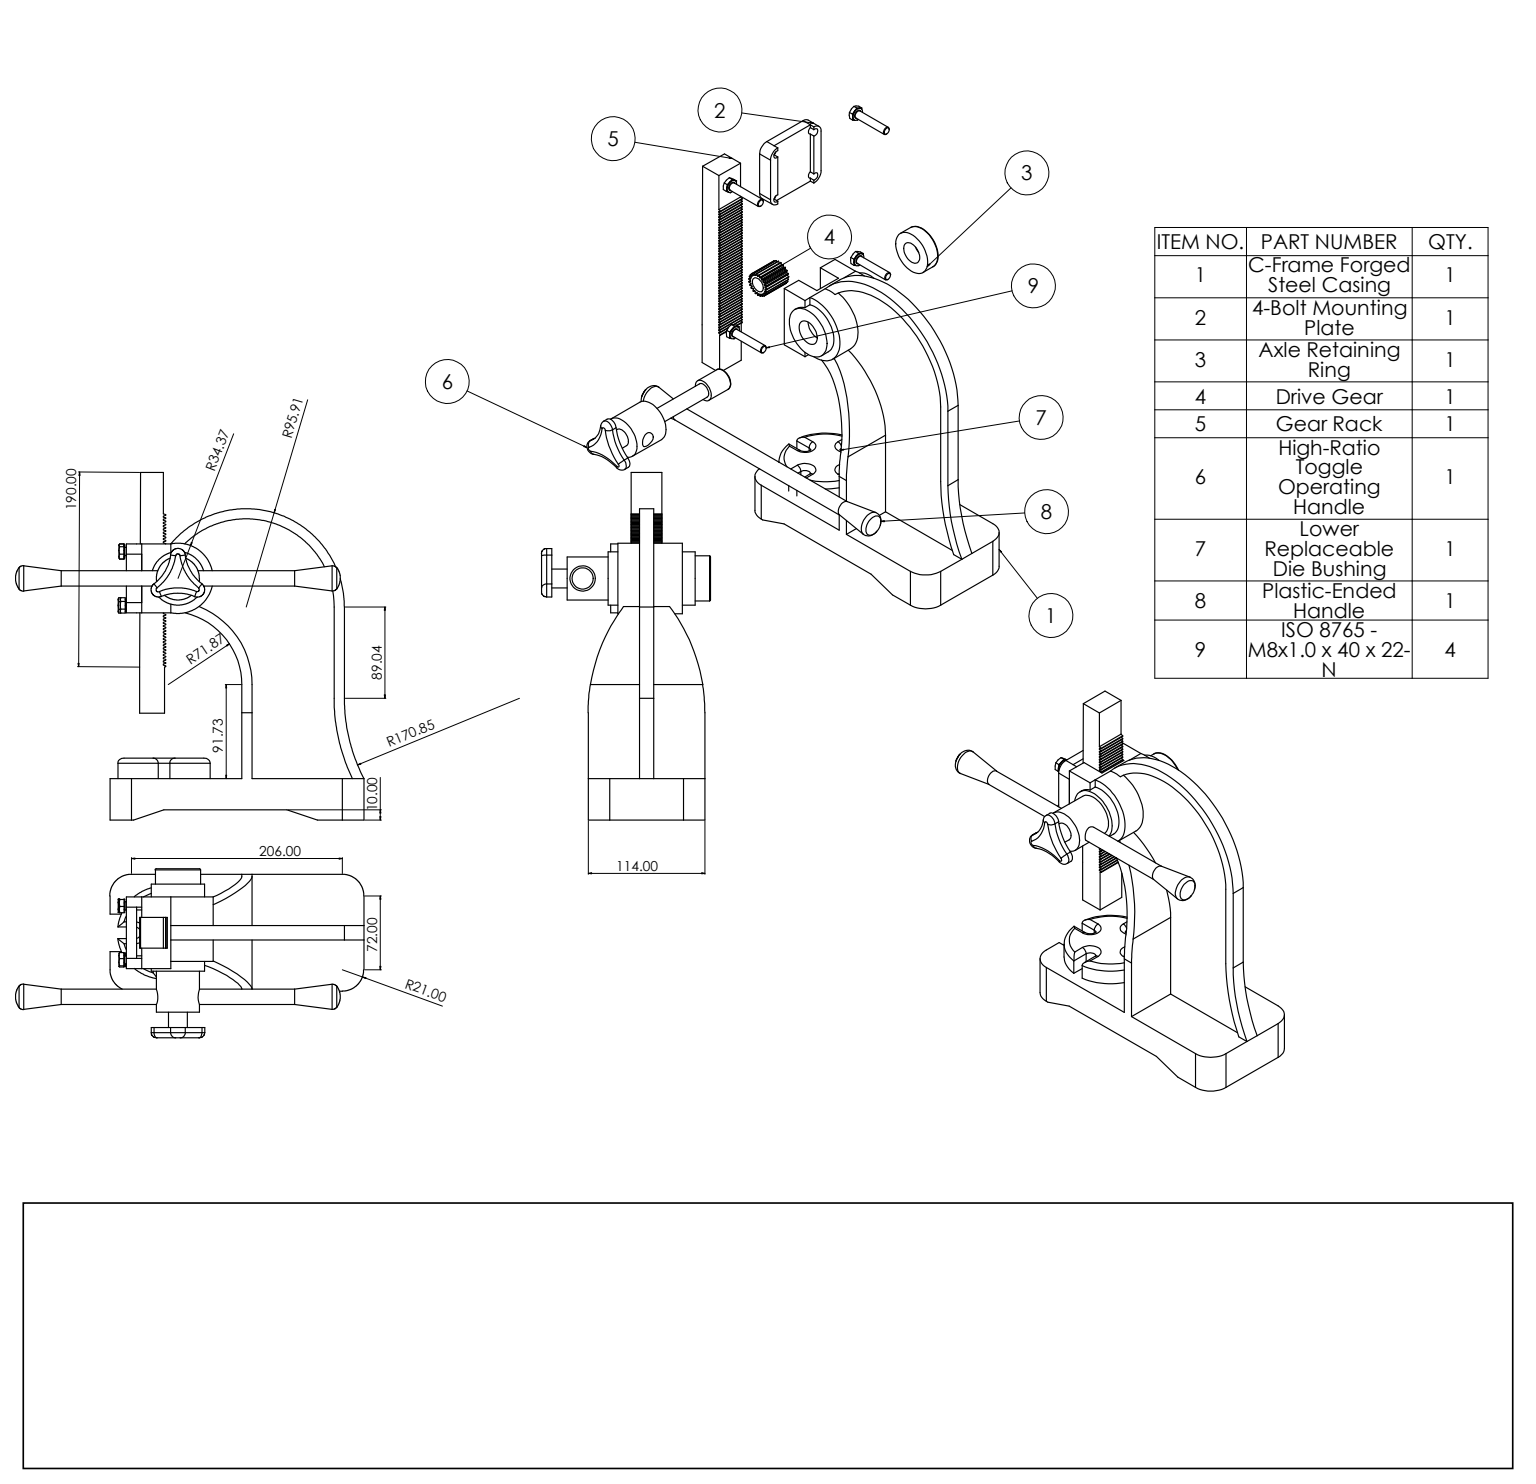
ISO-10303-21;
HEADER;
FILE_DESCRIPTION (('STEP AP214'),
    '1' );
FILE_NAME ('MAS-321',
    '2026-10-21T18:33:49',
    ( '' ),
    ( '' ),
    'SwSTEP 2.0',
    'SolidWorks 2025',
    '' );
FILE_SCHEMA (( 'AUTOMOTIVE_DESIGN' ));
ENDSEC;

DATA;
#1 = ORIENTED_EDGE ( 'NONE', *, *, #1823, .F. ) ;
#2 = EDGE_CURVE ( 'NONE', #15837, #10059, #9983, .T. ) ;
#3 = EDGE_CURVE ( 'NONE', #15101, #1867, #14100, .T. ) ;
#4 = VERTEX_POINT ( 'NONE', #5573 ) ;
#5 = DIRECTION ( 'NONE',  ( 0.000000000000000000, 1.000000000000000000, 0.000000000000000000 ) ) ;
#6 = CARTESIAN_POINT ( 'NONE',  ( 0.01372220897669153110, -5.309964801958256153, 3.802871176606155590 ) ) ;
#7 = CIRCLE ( 'NONE', #9259, 4.600000000000006750 ) ;
#8 = FACE_OUTER_BOUND ( 'NONE', #9764, .T. ) ;
#9 = EDGE_CURVE ( 'NONE', #4281, #6184, #12794, .T. ) ;
#10 = CARTESIAN_POINT ( 'NONE',  ( -68.99615306438082030, 67.98345733813023628, 15.00000000000006928 ) ) ;
#11 = AXIS2_PLACEMENT_3D ( 'NONE', #13563, #6445, #16272 ) ;
#12 = DIRECTION ( 'NONE',  ( -0.000000000000000000, -0.000000000000000000, -1.000000000000000000 ) ) ;
#13 = CIRCLE ( 'NONE', #606, 12.50000000000001776 ) ;
#14 = ORIENTED_EDGE ( 'NONE', *, *, #12006, .F. ) ;
#15 = ADVANCED_FACE ( 'NONE', ( #8489 ), #16983, .T. ) ;
#16 = DIRECTION ( 'NONE',  ( -5.204170427930409450E-16, 0.000000000000000000, 1.000000000000000000 ) ) ;
#17 = ORIENTED_EDGE ( 'NONE', *, *, #6060, .F. ) ;
#18 = CARTESIAN_POINT ( 'NONE',  ( -78.51801170372752381, -91.96846159163192169, 42.55230335834794175 ) ) ;
#19 = ADVANCED_FACE ( 'NONE', ( #15595 ), #11103, .T. ) ;
#20 = ADVANCED_FACE ( 'NONE', ( #8576 ), #7163, .T. ) ;
#21 = CARTESIAN_POINT ( 'NONE',  ( -67.50540723371459251, 87.07303407725210320, 15.00000000000006928 ) ) ;
#22 = ORIENTED_EDGE ( 'NONE', *, *, #922, .F. ) ;
#23 = VECTOR ( 'NONE', #5591, 1000.000000000000000 ) ;
#24 = CARTESIAN_POINT ( 'NONE',  ( -110.0337185876616815, -91.08930958056578220, -10.39386245929468444 ) ) ;
#25 = ORIENTED_EDGE ( 'NONE', *, *, #4430, .T. ) ;
#26 = AXIS2_PLACEMENT_3D ( 'NONE', #11599, #96, #9826 ) ;
#27 = ADVANCED_FACE ( 'NONE', ( #4362 ), #9999, .F. ) ;
#28 = VECTOR ( 'NONE', #11841, 1000.000000000000000 ) ;
#29 = VECTOR ( 'NONE', #2801, 1000.000000000000000 ) ;
#30 = EDGE_LOOP ( 'NONE', ( #4057, #14157, #6420, #5551 ) ) ;
#31 = SURFACE_STYLE_USAGE ( .BOTH. , #16764 ) ;
#32 = DIRECTION ( 'NONE',  ( -0.000000000000000000, -0.000000000000000000, -1.000000000000000000 ) ) ;
#33 = CARTESIAN_POINT ( 'NONE',  ( -68.99615306438083451, 95.64293533166268446, -15.00000000000001421 ) ) ;
#34 = ORIENTED_EDGE ( 'NONE', *, *, #18366, .F. ) ;
#35 = ITEM_DEFINED_TRANSFORMATION ( 'NONE', 'NONE', #15648,  #16217 ) ;
#36 = AXIS2_PLACEMENT_3D ( 'NONE', #1369, #138, #1266 ) ;
#37 = EDGE_LOOP ( 'NONE', ( #6433, #6306, #4816, #14039 ) ) ;
#38 = CARTESIAN_POINT ( 'NONE',  ( -27.30335599338096841, -92.58099833983887095, 7.070576347711331699 ) ) ;
#39 = DIRECTION ( 'NONE',  ( 3.469446951953611033E-15, 0.000000000000000000, -1.000000000000000000 ) ) ;
#40 = ORIENTED_EDGE ( 'NONE', *, *, #16480, .F. ) ;
#41 = LINE ( 'NONE', #15673, #2725 ) ;
#42 = DIRECTION ( 'NONE',  ( -1.000000000000000000, 5.416250486023790304E-15, 1.692578276882434470E-16 ) ) ;
#43 = CARTESIAN_POINT ( 'NONE',  ( -71.24615306438076345, 119.9567435045637609, 15.00000000000006928 ) ) ;
#44 = AXIS2_PLACEMENT_3D ( 'NONE', #11629, #14534, #15759 ) ;
#45 = AXIS2_PLACEMENT_3D ( 'NONE', #14996, #2189, #7901 ) ;
#46 = ORIENTED_EDGE ( 'NONE', *, *, #11434, .F. ) ;
#47 = EDGE_CURVE ( 'NONE', #3245, #18159, #14547, .T. ) ;
#48 = DIRECTION ( 'NONE',  ( -1.000000000000000000, 0.000000000000000000, 0.000000000000000000 ) ) ;
#49 = ORIENTED_EDGE ( 'NONE', *, *, #17445, .T. ) ;
#50 = ORIENTED_EDGE ( 'NONE', *, *, #8115, .F. ) ;
#51 = AXIS2_PLACEMENT_3D ( 'NONE', #16170, #17306, #13379 ) ;
#52 = DIRECTION ( 'NONE',  ( -1.000000000000000000, -0.000000000000000000, -0.000000000000000000 ) ) ;
#53 = ORIENTED_EDGE ( 'NONE', *, *, #16344, .F. ) ;
#54 = ORIENTED_EDGE ( 'NONE', *, *, #5988, .F. ) ;
#55 = CIRCLE ( 'NONE', #2439, 22.04359719766050318 ) ;
#56 = AXIS2_PLACEMENT_3D ( 'NONE', #11345, #9554, #17037 ) ;
#57 = DIRECTION ( 'NONE',  ( 0.000000000000000000, 0.000000000000000000, 1.000000000000000000 ) ) ;
#58 = DIRECTION ( 'NONE',  ( -1.000000000000000000, 0.000000000000000000, 1.156482317317869999E-16 ) ) ;
#59 = CARTESIAN_POINT ( 'NONE',  ( -71.24615306438080609, 110.5319655545637403, -15.00000000000001421 ) ) ;
#60 = VERTEX_POINT ( 'NONE', #5921 ) ;
#61 = CARTESIAN_POINT ( 'NONE',  ( -44.89980253466632831, 81.41924511788819530, 15.00000000000006928 ) ) ;
#62 = DIRECTION ( 'NONE',  ( 1.000000000000000000, 0.000000000000000000, 5.077734830647299712E-16 ) ) ;
#63 = CARTESIAN_POINT ( 'NONE',  ( -9.730036491473859073, 24.55694320255973651, 41.56001028271458608 ) ) ;
#64 = FACE_OUTER_BOUND ( 'NONE', #11864, .T. ) ;
#65 = ORIENTED_EDGE ( 'NONE', *, *, #13144, .F. ) ;
#66 = AXIS2_PLACEMENT_3D ( 'NONE', #17711, #16306, #507 ) ;
#67 = DIRECTION ( 'NONE',  ( 1.000000000000000000, 0.000000000000000000, 0.000000000000000000 ) ) ;
#68 = DIRECTION ( 'NONE',  ( 0.000000000000000000, 0.000000000000000000, -1.000000000000000000 ) ) ;
#69 = LINE ( 'NONE', #1924, #3643 ) ;
#70 = VERTEX_POINT ( 'NONE', #417 ) ;
#71 = CIRCLE ( 'NONE', #16786, 10.24900000000000055 ) ;
#72 = VECTOR ( 'NONE', #8079, 1000.000000000000000 ) ;
#73 = LINE ( 'NONE', #1738, #2546 ) ;
#74 = CARTESIAN_POINT ( 'NONE',  ( -71.24615306438114715, 12.25372266522925457, -15.00000000000001421 ) ) ;
#75 = CARTESIAN_POINT ( 'NONE',  ( -59.35080917176598092, 94.79374675277695417, -15.00000000000001421 ) ) ;
#76 = CARTESIAN_POINT ( 'NONE',  ( -68.99615306438099083, 39.70912348813027393, -15.00000000000001421 ) ) ;
#77 = ORIENTED_EDGE ( 'NONE', *, *, #12373, .F. ) ;
#78 = ORIENTED_EDGE ( 'NONE', *, *, #14054, .T. ) ;
#79 = VECTOR ( 'NONE', #3026, 1000.000000000000000 ) ;
#81 = ADVANCED_FACE ( 'NONE', ( #3143 ), #14460, .T. ) ;
#80 = FACE_OUTER_BOUND ( 'NONE', #8908, .T. ) ;
#82 = VECTOR ( 'NONE', #10770, 1000.000000000000000 ) ;
#83 = AXIS2_PLACEMENT_3D ( 'NONE', #305, #8649, #15842 ) ;
#84 = MANIFOLD_SOLID_BREP ( 'HeadFillet', #15945 ) ;
#85 =( NAMED_UNIT ( * ) SI_UNIT ( $, .STERADIAN. ) SOLID_ANGLE_UNIT ( ) );
#86 = CARTESIAN_POINT ( 'NONE',  ( -67.32681558843928826, 84.01587117655452630, 15.00000000000006928 ) ) ;
#87 = CARTESIAN_POINT ( 'NONE',  ( -71.24615306438086293, 87.65194626522927024, 15.00000000000006928 ) ) ;
#88 = CARTESIAN_POINT ( 'NONE',  ( -71.24615306438103346, 41.41692725456378099, 15.00000000000006928 ) ) ;
#89 = ORIENTED_EDGE ( 'NONE', *, *, #17144, .T. ) ;
#90 = DIRECTION ( 'NONE',  ( -0.000000000000000000, 0.000000000000000000, -1.000000000000000000 ) ) ;
#91 = LINE ( 'NONE', #5786, #7353 ) ;
#92 = FACE_OUTER_BOUND ( 'NONE', #4705, .T. ) ;
#93 = ORIENTED_EDGE ( 'NONE', *, *, #600, .F. ) ;
#94 = DIRECTION ( 'NONE',  ( 1.000000000000000000, 0.000000000000000000, -0.000000000000000000 ) ) ;
#95 = AXIS2_PLACEMENT_3D ( 'NONE', #13870, #16563, #957 ) ;
#96 = DIRECTION ( 'NONE',  ( -1.000000000000000000, -0.000000000000000000, -0.000000000000000000 ) ) ;
#97 = EDGE_LOOP ( 'NONE', ( #14559, #13719, #17905, #14362 ) ) ;
#98 = VECTOR ( 'NONE', #835, 1000.000000000000000 ) ;
#99 = CARTESIAN_POINT ( 'NONE',  ( -57.08002265617300708, 84.22855780814606419, 35.00000000000000000 ) ) ;
#100 = VECTOR ( 'NONE', #7999, 1000.000000000000000 ) ;
#101 = CARTESIAN_POINT ( 'NONE',  ( -71.24615306438103346, 46.81124181522922356, -167.1454815528550739 ) ) ;
#102 = ORIENTED_EDGE ( 'NONE', *, *, #5033, .T. ) ;
#103 = VERTEX_POINT ( 'NONE', #8932 ) ;
#104 = VECTOR ( 'NONE', #14107, 1000.000000000000000 ) ;
#105 = EDGE_CURVE ( 'NONE', #6184, #7713, #7257, .T. ) ;
#106 = DIRECTION ( 'NONE',  ( 0.000000000000000000, 0.000000000000000000, 1.000000000000000000 ) ) ;
#107 = CARTESIAN_POINT ( 'NONE',  ( -68.99615306438077766, 111.3508985816626335, 15.00000000000006928 ) ) ;
#108 = DIRECTION ( 'NONE',  ( 0.9396926207859110924, 0.3420201433256612189, 4.890320548438462711E-16 ) ) ;
#109 = CARTESIAN_POINT ( 'NONE',  ( -68.99615306438083451, 96.25779118813026969, 15.00000000000006928 ) ) ;
#110 = AXIS2_PLACEMENT_3D ( 'NONE', #2783, #3985, #15597 ) ;
#111 = AXIS2_PLACEMENT_3D ( 'NONE', #807, #12215, #17823 ) ;
#112 = CARTESIAN_POINT ( 'NONE',  ( -68.99615306438094819, 64.84186468813030046, -167.1454815528550739 ) ) ;
#113 = VERTEX_POINT ( 'NONE', #1813 ) ;
#114 = CARTESIAN_POINT ( 'NONE',  ( -57.08002265617300708, 84.22855780814606419, 15.00000000000006928 ) ) ;
#115 = VERTEX_POINT ( 'NONE', #11567 ) ;
#116 = EDGE_CURVE ( 'NONE', #6374, #8001, #17153, .T. ) ;
#117 = DIRECTION ( 'NONE',  ( 0.000000000000000000, 1.000000000000000000, -0.000000000000000000 ) ) ;
#118 = DIRECTION ( 'NONE',  ( 0.000000000000000000, -0.000000000000000000, 1.000000000000000000 ) ) ;
#120 = ADVANCED_FACE ( 'NONE', ( #317 ), #17523, .T. ) ;
#119 = ORIENTED_EDGE ( 'NONE', *, *, #16367, .F. ) ;
#121 = CARTESIAN_POINT ( 'NONE',  ( -115.7702289486887537, -95.65021661331556402, -5.654315315326000402 ) ) ;
#122 = ORIENTED_EDGE ( 'NONE', *, *, #17197, .T. ) ;
#123 = EDGE_CURVE ( 'NONE', #14184, #1161, #17431, .T. ) ;
#124 = AXIS2_PLACEMENT_3D ( 'NONE', #9916, #7194, #14307 ) ;
#125 = AXIS2_PLACEMENT_3D ( 'NONE', #2638, #18365, #4052 ) ;
#126 = ADVANCED_FACE ( 'NONE', ( #11640 ), #16856, .T. ) ;
#127 = ORIENTED_EDGE ( 'NONE', *, *, #11107, .F. ) ;
#128 = EDGE_CURVE ( 'NONE', #7354, #7590, #10341, .T. ) ;
#129 = FACE_OUTER_BOUND ( 'NONE', #15736, .T. ) ;
#130 = CYLINDRICAL_SURFACE ( 'NONE', #6082, 21.04359719766050318 ) ;
#131 = DIRECTION ( 'NONE',  ( 0.000000000000000000, 1.000000000000000000, 0.000000000000000000 ) ) ;
#132 = CLOSED_SHELL ( 'NONE', ( #16819, #11674, #2033, #11644, #4371, #4122, #1296, #5932, #17847, #120, #2885, #7783, #14078, #8551, #16458, #7777, #18333, #11455, #10717, #14761, #5893, #8655, #18440, #16557, #12743, #9060, #2113, #2878, #10557, #2402, #8018, #1483, #10883, #4144, #6355, #12130, #16320, #4815, #13864, #11004, #16568, #13389, #1952, #7426, #15874, #4708, #2702, #9166, #6647, #9938, #17322, #16215, #6855, #13752, #18352, #9497, #4258, #1742, #6653, #8457, #4789, #9269, #18511, #11812, #1620, #13520, #17365, #6946, #1859, #1613, #14320, #1393, #8249, #8120, #5145, #15892, #8683, #10886, #4488, #15641, #15634, #1683, #17355, #13695, #2863, #11359, #9380, #16584, #2602, #1587, #18091, #10091, #697, #5265, #11665, #1664, #1494, #15112, #7329, #13942, #12957, #5269, #13366, #4588, #17837, #11471, #8147, #8734, #4244, #11669, #7993, #15996, #11378, #16587, #15586, #9173, #1719, #9985, #9137, #3228, #3620, #3217, #7092, #3899, #10422, #4564, #11884, #18090, #10942, #9980, #5134, #5026, #2281, #4013, #13406, #12017, #13887, #8689, #14413, #199, #11412, #7110, #12033, #2993, #2286, #360, #17572, #10733, #12952, #12754, #9744, #1961, #13863, #8387, #17357, #7212, #8267, #16341, #10832, #3777, #7577, #14524, #13388, #3293, #4798, #16330, #4522, #14219, #18302, #4015, #3342, #248, #17345, #4135, #15214, #12844, #9850, #14995, #14426, #12814, #8137, #5256, #5374, #4240, #691, #4541, #672, #7328, #12390, #3982, #7563, #1284, #2154, #15527, #5570, #7390, #1348, #13976, #16311 ) ) ;
#133 = ORIENTED_EDGE ( 'NONE', *, *, #16066, .F. ) ;
#134 = CONTEXT_DEPENDENT_SHAPE_REPRESENTATION ( #8503, #15053 ) ;
#135 = ORIENTED_EDGE ( 'NONE', *, *, #18293, .T. ) ;
#136 = VECTOR ( 'NONE', #9589, 1000.000000000000000 ) ;
#137 = EDGE_CURVE ( 'NONE', #18033, #6955, #3220, .T. ) ;
#138 = DIRECTION ( 'NONE',  ( -0.000000000000000000, -0.000000000000000000, -1.000000000000000000 ) ) ;
#139 = CARTESIAN_POINT ( 'NONE',  ( -127.5926225674731711, 57.88796029049329661, -26.35917033480641436 ) ) ;
#140 = EDGE_CURVE ( 'NONE', #5342, #10434, #506, .T. ) ;
#141 = AXIS2_PLACEMENT_3D ( 'NONE', #1798, #14535, #303 ) ;
#142 = CARTESIAN_POINT ( 'NONE',  ( -71.24615306438106188, 35.13374195456378146, 15.00000000000006928 ) ) ;
#143 = CIRCLE ( 'NONE', #12708, 3.999999999999996447 ) ;
#144 = ADVANCED_FACE ( 'NONE', ( #11916 ), #17609, .T. ) ;
#145 = EDGE_LOOP ( 'NONE', ( #17261, #13971, #8851, #5219 ) ) ;
#146 = VECTOR ( 'NONE', #7240, 1000.000000000000114 ) ;
#147 = DIRECTION ( 'NONE',  ( 1.156482317317869999E-16, 0.000000000000000000, 1.000000000000000000 ) ) ;
#148 = ORIENTED_EDGE ( 'NONE', *, *, #2746, .F. ) ;
#149 = ORIENTED_EDGE ( 'NONE', *, *, #11735, .T. ) ;
#150 = EDGE_CURVE ( 'NONE', #4219, #3665, #3494, .T. ) ;
#151 = COLOUR_RGB ( '',0.7921568627450980005, 0.8196078431372548767, 0.9333333333333333481 ) ;
#152 = MANIFOLD_SOLID_BREP ( 'Revolve1', #15042 ) ;
#153 = ORIENTED_EDGE ( 'NONE', *, *, #7643, .F. ) ;
#154 = AXIS2_PLACEMENT_3D ( 'NONE', #13342, #6302, #517 ) ;
#155 = AXIS2_PLACEMENT_3D ( 'NONE', #551, #8645, #16166 ) ;
#156 = EDGE_CURVE ( 'NONE', #14603, #10461, #7800, .T. ) ;
#157 = CIRCLE ( 'NONE', #3134, 10.38004356723770627 ) ;
#158 = DIRECTION ( 'NONE',  ( 0.000000000000000000, 0.000000000000000000, -1.000000000000000000 ) ) ;
#159 = EDGE_CURVE ( 'NONE', #3245, #14275, #15961, .T. ) ;
#160 = CARTESIAN_POINT ( 'NONE',  ( -68.99615306438087714, 64.84186468813027204, 15.00000000000006928 ) ) ;
#161 = LINE ( 'NONE', #5851, #4306 ) ;
#162 = VERTEX_POINT ( 'NONE', #5272 ) ;
#163 = CARTESIAN_POINT ( 'NONE',  ( -71.24615306438072082, 129.3815214545637104, -15.00000000000001421 ) ) ;
#164 = DIRECTION ( 'NONE',  ( -1.000000000000000000, 0.000000000000000000, 0.000000000000000000 ) ) ;
#165 = DIRECTION ( 'NONE',  ( 0.000000000000000000, 1.000000000000000000, 0.000000000000000000 ) ) ;
#166 = PLANE ( 'NONE',  #9698 ) ;
#167 = ORIENTED_EDGE ( 'NONE', *, *, #3319, .T. ) ;
#168 = DIRECTION ( 'NONE',  ( 0.000000000000000000, -1.000000000000000000, 0.000000000000000000 ) ) ;
#169 = CARTESIAN_POINT ( 'NONE',  ( -59.35080917176598092, 94.79374675277695417, 15.00000000000006928 ) ) ;
#170 = FACE_OUTER_BOUND ( 'NONE', #6777, .T. ) ;
#171 = EDGE_LOOP ( 'NONE', ( #9125, #326, #2269 ) ) ;
#172 = VECTOR ( 'NONE', #13804, 1000.000000000000000 ) ;
#173 = VECTOR ( 'NONE', #14749, 1000.000000000000000 ) ;
#174 = VECTOR ( 'NONE', #6629, 999.9999999999998863 ) ;
#175 = DIRECTION ( 'NONE',  ( 1.000000000000000000, 0.000000000000000000, 0.000000000000000000 ) ) ;
#176 = DIRECTION ( 'NONE',  ( 0.000000000000000000, 1.000000000000000000, 0.000000000000000000 ) ) ;
#177 = ORIENTED_EDGE ( 'NONE', *, *, #14769, .T. ) ;
#178 = EDGE_LOOP ( 'NONE', ( #16402, #10742, #3348, #2661 ) ) ;
#179 = DIRECTION ( 'NONE',  ( 1.000000000000000000, 0.000000000000000000, 5.551115123125780730E-16 ) ) ;
#180 = CIRCLE ( 'NONE', #10627, 4.025000000000000355 ) ;
#181 = SHAPE_REPRESENTATION_RELATIONSHIP ( 'NONE' , 'NONE' ,  #5501, #12175 ) ;
#182 = VECTOR ( 'NONE', #7830, 1000.000000000000000 ) ;
#183 = CARTESIAN_POINT ( 'NONE',  ( -70.85175816390371040, -141.5628872026273086, -18.23991632971910803 ) ) ;
#184 = CARTESIAN_POINT ( 'NONE',  ( -64.80066835027049876, -94.42547236494613117, -44.74948972093426391 ) ) ;
#185 = ORIENTED_EDGE ( 'NONE', *, *, #7525, .T. ) ;
#186 = CARTESIAN_POINT ( 'NONE',  ( 49.38736944425944841, -141.5628872026273086, -57.00000000000000000 ) ) ;
#187 = DIRECTION ( 'NONE',  ( -5.204170427930409450E-16, 0.000000000000000000, 1.000000000000000000 ) ) ;
#188 = DIRECTION ( 'NONE',  ( 0.000000000000000000, 0.000000000000000000, 1.000000000000000000 ) ) ;
#189 = DIRECTION ( 'NONE',  ( -0.9396926207859084279, 0.3420201433256686574, -4.890320548438448905E-16 ) ) ;
#190 = ORIENTED_EDGE ( 'NONE', *, *, #16753, .F. ) ;
#191 = DIRECTION ( 'NONE',  ( 1.156482317317869999E-16, 0.000000000000000000, 1.000000000000000000 ) ) ;
#192 = CYLINDRICAL_SURFACE ( 'NONE', #914, 11.04359719766050141 ) ;
#193 = EDGE_LOOP ( 'NONE', ( #119, #17076, #7928, #5091 ) ) ;
#194 = PRODUCT_RELATED_PRODUCT_CATEGORY ( 'part', '', ( #10574 ) ) ;
#195 = CYLINDRICAL_SURFACE ( 'NONE', #16432, 4.599999999999999645 ) ;
#196 = CARTESIAN_POINT ( 'NONE',  ( -93.73308511844572877, 147.7866419848965052, 15.00000000000006928 ) ) ;
#197 = VERTEX_POINT ( 'NONE', #9569 ) ;
#198 = ORIENTED_EDGE ( 'NONE', *, *, #17480, .F. ) ;
#199 = ADVANCED_FACE ( 'NONE', ( #6677 ), #6475, .T. ) ;
#200 = ORIENTED_EDGE ( 'NONE', *, *, #18072, .T. ) ;
#201 = DIRECTION ( 'NONE',  ( -1.000000000000000000, 2.331468351712825579E-14, 1.387778780781443703E-16 ) ) ;
#202 = LINE ( 'NONE', #14676, #5765 ) ;
#203 = FACE_OUTER_BOUND ( 'NONE', #17910, .T. ) ;
#204 = FACE_OUTER_BOUND ( 'NONE', #12195, .T. ) ;
#205 = CARTESIAN_POINT ( 'NONE',  ( -64.09025127992788384, 50.58224449241410525, 35.00000000000000000 ) ) ;
#206 = ORIENTED_EDGE ( 'NONE', *, *, #10760, .F. ) ;
#207 = CARTESIAN_POINT ( 'NONE',  ( -68.99615306438072082, 139.6252324316626812, -15.00000000000001421 ) ) ;
#208 = CARTESIAN_POINT ( 'NONE',  ( -80.32997185471272417, -91.18731257919070288, 40.31990080433438095 ) ) ;
#209 = DIRECTION ( 'NONE',  ( 1.156482317317869999E-16, 0.000000000000000000, 1.000000000000000000 ) ) ;
#210 = ORIENTED_EDGE ( 'NONE', *, *, #16102, .F. ) ;
#211 = CARTESIAN_POINT ( 'NONE',  ( -71.24615306438094819, 65.66079771522920794, 15.00000000000006928 ) ) ;
#212 = CARTESIAN_POINT ( 'NONE',  ( -114.8884567811962967, -93.39009998357855125, -6.425136209964025902 ) ) ;
#213 = ORIENTED_EDGE ( 'NONE', *, *, #3679, .F. ) ;
#214 = EDGE_LOOP ( 'NONE', ( #597, #4033, #2043, #6029 ) ) ;
#215 = ADVANCED_FACE ( 'NONE', ( #695 ), #10288, .T. ) ;
#216 = DIRECTION ( 'NONE',  ( 0.000000000000000000, 0.000000000000000000, 1.000000000000000000 ) ) ;
#217 = CARTESIAN_POINT ( 'NONE',  ( -97.59262256747317110, 0.3328663868096687350, 25.00000000000000000 ) ) ;
#218 = DIRECTION ( 'NONE',  ( 0.000000000000000000, 0.000000000000000000, 1.000000000000000000 ) ) ;
#219 = ORIENTED_EDGE ( 'NONE', *, *, #12477, .T. ) ;
#220 = ORIENTED_EDGE ( 'NONE', *, *, #11450, .F. ) ;
#221 = CARTESIAN_POINT ( 'NONE',  ( -81.37409655828265898, -96.08423613455721579, -2.623087607583323579E-13 ) ) ;
#222 = FACE_OUTER_BOUND ( 'NONE', #11208, .T. ) ;
#223 = DIRECTION ( 'NONE',  ( 0.000000000000000000, -0.000000000000000000, 1.000000000000000000 ) ) ;
#224 = CARTESIAN_POINT ( 'NONE',  ( -68.99615306438066398, 143.3816809381303585, -15.00000000000001421 ) ) ;
#225 = ORIENTED_EDGE ( 'NONE', *, *, #7011, .F. ) ;
#226 = EDGE_CURVE ( 'NONE', #10713, #3636, #7893, .T. ) ;
#227 = DIRECTION ( 'NONE',  ( 1.000000000000000000, 0.000000000000000000, 0.000000000000000000 ) ) ;
#228 = ORIENTED_EDGE ( 'NONE', *, *, #586, .F. ) ;
#229 = EDGE_CURVE ( 'NONE', #6748, #3936, #16550, .T. ) ;
#230 = EDGE_LOOP ( 'NONE', ( #6684, #5867, #2533, #3953 ) ) ;
#231 = ORIENTED_EDGE ( 'NONE', *, *, #17262, .F. ) ;
#232 = EDGE_CURVE ( 'NONE', #7225, #15152, #10982, .T. ) ;
#233 = EDGE_CURVE ( 'NONE', #4074, #17713, #2000, .T. ) ;
#234 = DIRECTION ( 'NONE',  ( 0.000000000000000000, 0.000000000000000000, 1.000000000000000000 ) ) ;
#235 = CARTESIAN_POINT ( 'NONE',  ( -68.99615306438097662, 57.94382353166266597, 15.00000000000006928 ) ) ;
#236 = ORIENTED_EDGE ( 'NONE', *, *, #5271, .F. ) ;
#237 = CYLINDRICAL_SURFACE ( 'NONE', #286, 4.599999999999999645 ) ;
#238 = CARTESIAN_POINT ( 'NONE',  ( -68.99615306438094819, 52.27549408813023746, -15.00000000000001421 ) ) ;
#239 = CARTESIAN_POINT ( 'NONE',  ( -68.99615306438091977, 76.79337943166271430, 15.00000000000006928 ) ) ;
#240 = DIRECTION ( 'NONE',  ( 1.000000000000000000, 0.000000000000000000, 0.000000000000000000 ) ) ;
#241 = ORIENTED_EDGE ( 'NONE', *, *, #15088, .F. ) ;
#242 = EDGE_CURVE ( 'NONE', #13281, #15993, #13414, .T. ) ;
#243 = CARTESIAN_POINT ( 'NONE',  ( 0.000000000000000000, -47.21335801510345220, 0.000000000000000000 ) ) ;
#244 = EDGE_CURVE ( 'NONE', #4575, #11504, #16586, .T. ) ;
#245 = DIRECTION ( 'NONE',  ( 0.000000000000000000, 1.000000000000000000, 0.000000000000000000 ) ) ;
#246 = CARTESIAN_POINT ( 'NONE',  ( -68.99615306438089135, 67.36860148166267948, -15.00000000000001421 ) ) ;
#247 = EDGE_LOOP ( 'NONE', ( #1699, #2209, #13687, #4336 ) ) ;
#248 = ADVANCED_FACE ( 'NONE', ( #16665 ), #17710, .T. ) ;
#249 = CYLINDRICAL_SURFACE ( 'NONE', #1928, 10.24900000000000766 ) ;
#250 = EDGE_CURVE ( 'NONE', #2407, #15787, #4070, .T. ) ;
#251 = AXIS2_PLACEMENT_3D ( 'NONE', #13885, #4066, #1079 ) ;
#252 = DIRECTION ( 'NONE',  ( 0.000000000000000000, 0.000000000000000000, 1.000000000000000000 ) ) ;
#253 = EDGE_LOOP ( 'NONE', ( #10457, #6808, #9246, #11912 ) ) ;
#254 = EDGE_LOOP ( 'NONE', ( #4957, #10703, #17741, #2803 ) ) ;
#255 = EDGE_CURVE ( 'NONE', #17238, #6285, #13006, .T. ) ;
#256 = DIRECTION ( 'NONE',  ( 0.000000000000000000, 0.000000000000000000, 1.000000000000000000 ) ) ;
#257 = MANIFOLD_SOLID_BREP ( 'Fillet4', #11497 ) ;
#258 = DIRECTION ( 'NONE',  ( 1.000000000000000000, 0.000000000000000000, 0.000000000000000000 ) ) ;
#259 = CARTESIAN_POINT ( 'NONE',  ( -49.58002265617300708, 84.22855780814606419, 35.00000000000000000 ) ) ;
#260 = DIRECTION ( 'NONE',  ( 1.000000000000000000, 0.000000000000000000, 0.000000000000000000 ) ) ;
#261 = VECTOR ( 'NONE', #17294, 1000.000000000000000 ) ;
#262 = CARTESIAN_POINT ( 'NONE',  ( -92.59262256747321373, 107.8748711238780373, 25.00000000000000000 ) ) ;
#263 = ORIENTED_EDGE ( 'NONE', *, *, #18181, .T. ) ;
#264 = CYLINDRICAL_SURFACE ( 'NONE', #16430, 21.04359719766050318 ) ;
#265 = DIRECTION ( 'NONE',  ( 0.000000000000000000, 0.000000000000000000, 1.000000000000000000 ) ) ;
#266 = CARTESIAN_POINT ( 'NONE',  ( -37.39678785461407529, 56.02900023377289074, 23.03959524935876857 ) ) ;
#267 = CARTESIAN_POINT ( 'NONE',  ( -38.92363814577095837, 71.26406042838981136, 102.5000000000000000 ) ) ;
#268 = DIRECTION ( 'NONE',  ( -0.000000000000000000, -0.000000000000000000, -1.000000000000000000 ) ) ;
#269 = DIRECTION ( 'NONE',  ( 0.000000000000000000, -2.775557561562874095E-16, 1.000000000000000000 ) ) ;
#270 = ORIENTED_EDGE ( 'NONE', *, *, #16707, .F. ) ;
#271 = CARTESIAN_POINT ( 'NONE',  ( -66.92930002414082935, 60.44851893123529152, 25.00000000000000000 ) ) ;
#272 = CARTESIAN_POINT ( 'NONE',  ( -67.13262496892538422, 91.65790412808873100, -167.1454815528550739 ) ) ;
#273 = ORIENTED_EDGE ( 'NONE', *, *, #7918, .F. ) ;
#274 = VERTEX_POINT ( 'NONE', #11460 ) ;
#275 = ORIENTED_EDGE ( 'NONE', *, *, #8832, .T. ) ;
#276 = LINE ( 'NONE', #12841, #12086 ) ;
#277 = CARTESIAN_POINT ( 'NONE',  ( -71.24615306438070661, 137.9174286652292096, -15.00000000000001421 ) ) ;
#278 = CARTESIAN_POINT ( 'NONE',  ( -68.99615306438091977, 76.79337943166271430, 15.00000000000006928 ) ) ;
#279 = DIRECTION ( 'NONE',  ( -0.9396926207859097602, 0.3420201433256649937, 1.086737899652991371E-16 ) ) ;
#280 = CARTESIAN_POINT ( 'NONE',  ( -93.73308511844572877, 147.7866419848965052, -167.1454815528550739 ) ) ;
#281 = CARTESIAN_POINT ( 'NONE',  ( -71.24615306438117557, 2.828944715229236628, -15.00000000000001421 ) ) ;
#282 = ORIENTED_EDGE ( 'NONE', *, *, #10987, .T. ) ;
#283 = AXIS2_PLACEMENT_3D ( 'NONE', #4428, #227, #10141 ) ;
#284 = DIRECTION ( 'NONE',  ( 0.000000000000000000, 0.000000000000000000, 1.000000000000000000 ) ) ;
#285 = CARTESIAN_POINT ( 'NONE',  ( -80.85270481229034090, -91.10977358899566525, 39.65137850708985923 ) ) ;
#286 = AXIS2_PLACEMENT_3D ( 'NONE', #17181, #15858, #14286 ) ;
#287 = CARTESIAN_POINT ( 'NONE',  ( -71.24615306438091977, 78.22716831522920700, -167.1454815528550739 ) ) ;
#288 = VERTEX_POINT ( 'NONE', #1257 ) ;
#289 = LINE ( 'NONE', #11809, #4058 ) ;
#290 = DIRECTION ( 'NONE',  ( 0.000000000000000000, 1.000000000000000000, -0.000000000000000000 ) ) ;
#291 = ORIENTED_EDGE ( 'NONE', *, *, #13628, .T. ) ;
#292 = VECTOR ( 'NONE', #17881, 1000.000000000000000 ) ;
#293 = VERTEX_POINT ( 'NONE', #8174 ) ;
#294 = AXIS2_PLACEMENT_3D ( 'NONE', #10449, #2985, #15881 ) ;
#295 = DIRECTION ( 'NONE',  ( 1.000000000000000000, 0.000000000000000000, 3.771137991253934490E-16 ) ) ;
#296 = LINE ( 'NONE', #5733, #146 ) ;
#297 = EDGE_CURVE ( 'NONE', #9307, #9072, #17170, .T. ) ;
#298 = LINE ( 'NONE', #4419, #17998 ) ;
#299 = VERTEX_POINT ( 'NONE', #17149 ) ;
#300 = ORIENTED_EDGE ( 'NONE', *, *, #349, .T. ) ;
#301 = DIRECTION ( 'NONE',  ( 0.000000000000000000, 0.000000000000000000, -1.000000000000000000 ) ) ;
#302 = CARTESIAN_POINT ( 'NONE',  ( 105.4583593777967963, -32.62665103886256190, -7.000000000000010658 ) ) ;
#303 = DIRECTION ( 'NONE',  ( -0.9396926207859083169, 0.3420201433256687129, 0.000000000000000000 ) ) ;
#304 = VECTOR ( 'NONE', #7741, 1000.000000000000000 ) ;
#305 = CARTESIAN_POINT ( 'NONE',  ( -56.26901274438541378, 73.45256821284058901, -15.00000000000001421 ) ) ;
#306 = ORIENTED_EDGE ( 'NONE', *, *, #1227, .F. ) ;
#307 = CIRCLE ( 'NONE', #13165, 4.962965561209093046 ) ;
#308 = PLANE ( 'NONE',  #11935 ) ;
#309 = EDGE_CURVE ( 'NONE', #9564, #16752, #11785, .T. ) ;
#310 = ORIENTED_EDGE ( 'NONE', *, *, #17032, .T. ) ;
#311 = EDGE_CURVE ( 'NONE', #17138, #8972, #12775, .T. ) ;
#312 = AXIS2_PLACEMENT_3D ( 'NONE', #18500, #6897, #18319 ) ;
#313 = ORIENTED_EDGE ( 'NONE', *, *, #10756, .F. ) ;
#314 = MANIFOLD_SOLID_BREP ( 'Cut-Extrude8', #12995 ) ;
#315 = VERTEX_POINT ( 'NONE', #4152 ) ;
#316 = VECTOR ( 'NONE', #2722, 1000.000000000000000 ) ;
#317 = FACE_OUTER_BOUND ( 'NONE', #5144, .T. ) ;
#318 = AXIS2_PLACEMENT_3D ( 'NONE', #739, #6431, #16426 ) ;
#319 = FACE_BOUND ( 'NONE', #1203, .T. ) ;
#320 = LINE ( 'NONE', #12982, #15345 ) ;
#321 = EDGE_LOOP ( 'NONE', ( #11496, #14503 ) ) ;
#322 = AXIS2_PLACEMENT_3D ( 'NONE', #3585, #3405, #3694 ) ;
#323 = DIRECTION ( 'NONE',  ( 0.000000000000000000, 0.000000000000000000, -1.000000000000000000 ) ) ;
#324 = FACE_OUTER_BOUND ( 'NONE', #5532, .T. ) ;
#325 = CARTESIAN_POINT ( 'NONE',  ( -69.66239992860627694, 84.22855780814606419, 37.50000000000000000 ) ) ;
#326 = ORIENTED_EDGE ( 'NONE', *, *, #2755, .T. ) ;
#327 = CARTESIAN_POINT ( 'NONE',  ( -71.24615306438086293, 101.1071876045637055, 15.00000000000006928 ) ) ;
#328 = CYLINDRICAL_SURFACE ( 'NONE', #16782, 4.599999999999999645 ) ;
#329 = DIRECTION ( 'NONE',  ( 1.156482317317869999E-16, 0.000000000000000000, 1.000000000000000000 ) ) ;
#330 = ORIENTED_EDGE ( 'NONE', *, *, #16668, .T. ) ;
#331 = EDGE_CURVE ( 'NONE', #1479, #11856, #14263, .T. ) ;
#332 = AXIS2_PLACEMENT_3D ( 'NONE', #14799, #4971, #14887 ) ;
#333 = EDGE_CURVE ( 'NONE', #677, #12056, #6961, .T. ) ;
#334 = CARTESIAN_POINT ( 'NONE',  ( -107.5926225674731853, 110.5691553257988460, 22.33417033480641223 ) ) ;
#335 = EDGE_CURVE ( 'NONE', #5779, #10128, #2839, .T. ) ;
#336 = CARTESIAN_POINT ( 'NONE',  ( 0.000000000000000000, -111.0842361345572158, 0.000000000000000000 ) ) ;
#337 = AXIS2_PLACEMENT_3D ( 'NONE', #17527, #14630, #13242 ) ;
#338 = ORIENTED_EDGE ( 'NONE', *, *, #1743, .T. ) ;
#339 = ORIENTED_EDGE ( 'NONE', *, *, #18046, .F. ) ;
#340 = ADVANCED_FACE ( 'NONE', ( #13312 ), #13217, .T. ) ;
#341 = EDGE_LOOP ( 'NONE', ( #13382, #1827, #3873, #1999 ) ) ;
#342 = EDGE_CURVE ( 'NONE', #6852, #6867, #8831, .T. ) ;
#343 = DIRECTION ( 'NONE',  ( -0.000000000000000000, -1.000000000000000000, 0.000000000000000000 ) ) ;
#344 = EDGE_CURVE ( 'NONE', #16643, #10257, #17318, .T. ) ;
#345 = ORIENTED_EDGE ( 'NONE', *, *, #13737, .F. ) ;
#346 = LINE ( 'NONE', #14229, #2566 ) ;
#347 = SHAPE_REPRESENTATION_RELATIONSHIP ( 'NONE' , 'NONE' ,  #8623, #5245 ) ;
#348 = CARTESIAN_POINT ( 'NONE',  ( -65.94558993203320085, 89.37090336996871542, -167.1454815528550739 ) ) ;
#349 = EDGE_CURVE ( 'NONE', #6911, #16349, #396, .T. ) ;
#350 = CARTESIAN_POINT ( 'NONE',  ( -83.23321842955245131, 73.26749283226919829, 97.49999999999998579 ) ) ;
#351 = ORIENTED_EDGE ( 'NONE', *, *, #16581, .T. ) ;
#352 = DIRECTION ( 'NONE',  ( 1.000000000000000000, 0.000000000000000000, 0.000000000000000000 ) ) ;
#353 = AXIS2_PLACEMENT_3D ( 'NONE', #9432, #13643, #6427 ) ;
#354 = AXIS2_PLACEMENT_3D ( 'NONE', #17589, #6266, #16189 ) ;
#355 = FACE_OUTER_BOUND ( 'NONE', #8735, .T. ) ;
#356 = LINE ( 'NONE', #17469, #14795 ) ;
#357 = CARTESIAN_POINT ( 'NONE',  ( -57.08002265617300708, 84.22855780814606419, 37.50000000000000000 ) ) ;
#358 = CARTESIAN_POINT ( 'NONE',  ( -37.24050225201523290, 91.24541864506342392, 59.84040329251897816 ) ) ;
#359 = SHAPE_REPRESENTATION ( 'MAS-321', ( #11759, #12682, #6990, #16528, #5173, #15648, #1001, #16837, #18016, #7567, #17423, #1327, #12362 ), #6356 ) ;
#360 = ADVANCED_FACE ( 'NONE', ( #11718 ), #4683, .T. ) ;
#361 = ADVANCED_FACE ( 'NONE', ( #3024 ), #9005, .T. ) ;
#362 = EDGE_CURVE ( 'NONE', #16861, #16195, #8816, .T. ) ;
#363 = LINE ( 'NONE', #13186, #2716 ) ;
#364 = EDGE_LOOP ( 'NONE', ( #17923, #6580, #8232, #7279 ) ) ;
#365 = VECTOR ( 'NONE', #12626, 1000.000000000000000 ) ;
#366 = EDGE_CURVE ( 'NONE', #16976, #11956, #1702, .T. ) ;
#367 = CARTESIAN_POINT ( 'NONE',  ( -66.14751942900640813, 58.73266222548429027, 25.00000000000001066 ) ) ;
#368 =( LENGTH_UNIT ( ) NAMED_UNIT ( * ) SI_UNIT ( .MILLI., .METRE. ) );
#369 = ORIENTED_EDGE ( 'NONE', *, *, #4474, .F. ) ;
#370 = ORIENTED_EDGE ( 'NONE', *, *, #2385, .F. ) ;
#371 = AXIS2_PLACEMENT_3D ( 'NONE', #10964, #16647, #17683 ) ;
#372 = EDGE_LOOP ( 'NONE', ( #7742, #5661, #16335, #12943 ) ) ;
#373 = ADVANCED_FACE ( 'NONE', ( #129 ), #745, .T. ) ;
#374 = CARTESIAN_POINT ( 'NONE',  ( -212.2032458117903104, 84.22855780814606419, 52.11995643276230794 ) ) ;
#375 = CYLINDRICAL_SURFACE ( 'NONE', #9052, 85.91469608272775815 ) ;
#376 = EDGE_CURVE ( 'NONE', #3236, #18474, #3199, .T. ) ;
#377 = CARTESIAN_POINT ( 'NONE',  ( -77.86181869377003295, 80.88798785482902076, 69.23289521281527925 ) ) ;
#378 = CARTESIAN_POINT ( 'NONE',  ( -71.20965894365861004, 109.9770744052236324, 22.40029077787859890 ) ) ;
#379 = AXIS2_PLACEMENT_3D ( 'NONE', #9478, #9862, #8069 ) ;
#380 = CARTESIAN_POINT ( 'NONE',  ( -81.37409655828265898, -96.08423613455721579, -8.525034724645805924E-13 ) ) ;
#381 = DIRECTION ( 'NONE',  ( 0.9396926207859097602, 0.3420201433256649937, -1.086737899652991371E-16 ) ) ;
#382 = ORIENTED_EDGE ( 'NONE', *, *, #14734, .F. ) ;
#383 = DIRECTION ( 'NONE',  ( 0.000000000000000000, 1.000000000000000000, 0.000000000000000000 ) ) ;
#384 = DIRECTION ( 'NONE',  ( -0.000000000000000000, 1.000000000000000000, -1.200240087506842815E-16 ) ) ;
#385 = VECTOR ( 'NONE', #2920, 999.9999999999998863 ) ;
#386 = VECTOR ( 'NONE', #13903, 1000.000000000000000 ) ;
#387 = DIRECTION ( 'NONE',  ( 0.000000000000000000, 1.000000000000000000, 0.000000000000000000 ) ) ;
#388 = ORIENTED_EDGE ( 'NONE', *, *, #15999, .F. ) ;
#389 = DIRECTION ( 'NONE',  ( 0.000000000000000000, 0.000000000000000000, 1.000000000000000000 ) ) ;
#390 = DIRECTION ( 'NONE',  ( 0.000000000000000000, 0.000000000000000000, 1.000000000000000000 ) ) ;
#391 = ORIENTED_EDGE ( 'NONE', *, *, #17491, .F. ) ;
#392 = ORIENTED_EDGE ( 'NONE', *, *, #13744, .T. ) ;
#393 = AXIS2_PLACEMENT_3D ( 'NONE', #6338, #7848, #6238 ) ;
#394 = CIRCLE ( 'NONE', #2180, 3.999999999999982681 ) ;
#395 = AXIS2_PLACEMENT_3D ( 'NONE', #4110, #9813, #15514 ) ;
#396 = LINE ( 'NONE', #4417, #4324 ) ;
#397 = CARTESIAN_POINT ( 'NONE',  ( -50.06979403241810900, 50.58224449241409104, -26.91246033477409583 ) ) ;
#398 = LINE ( 'NONE', #4246, #4265 ) ;
#399 = ORIENTED_EDGE ( 'NONE', *, *, #757, .T. ) ;
#400 = CARTESIAN_POINT ( 'NONE',  ( -28.16748190072492974, -91.96845925178433845, 7.798233810088259332 ) ) ;
#401 = VERTEX_POINT ( 'NONE', #7407 ) ;
#402 = AXIS2_PLACEMENT_3D ( 'NONE', #10590, #6260, #12088 ) ;
#403 = DIRECTION ( 'NONE',  ( -0.9396926207859103153, 0.3420201433256634949, -4.890320548438458766E-16 ) ) ;
#404 = LINE ( 'NONE', #6368, #15281 ) ;
#405 = DIRECTION ( 'NONE',  ( 1.000000000000000000, 0.000000000000000000, 0.000000000000000000 ) ) ;
#406 = DIRECTION ( 'NONE',  ( 0.000000000000000000, 0.000000000000000000, 1.000000000000000000 ) ) ;
#407 = ORIENTED_EDGE ( 'NONE', *, *, #6384, .T. ) ;
#408 = LINE ( 'NONE', #4696, #15529 ) ;
#409 = VERTEX_POINT ( 'NONE', #8909 ) ;
#410 = VECTOR ( 'NONE', #11298, 1000.000000000000000 ) ;
#411 = FACE_OUTER_BOUND ( 'NONE', #8890, .T. ) ;
#413 = ORIENTED_EDGE ( 'NONE', *, *, #7885, .T. ) ;
#412 = AXIS2_PLACEMENT_3D ( 'NONE', #18211, #5379, #6987 ) ;
#414 = EDGE_CURVE ( 'NONE', #2953, #996, #7597, .T. ) ;
#415 = VERTEX_POINT ( 'NONE', #17506 ) ;
#416 = EDGE_CURVE ( 'NONE', #17198, #9318, #10399, .T. ) ;
#417 = CARTESIAN_POINT ( 'NONE',  ( -50.35400969968294049, 73.69239390902568232, 15.00000000000006928 ) ) ;
#418 = CARTESIAN_POINT ( 'NONE',  ( -71.24615306438117557, 6.859408104563785358, -15.00000000000001421 ) ) ;
#419 = ORIENTED_EDGE ( 'NONE', *, *, #16175, .T. ) ;
#420 = VECTOR ( 'NONE', #9508, 1000.000000000000000 ) ;
#422 = VECTOR ( 'NONE', #7146, 1000.000000000000000 ) ;
#421 = DIRECTION ( 'NONE',  ( -1.000000000000000000, 0.000000000000000000, 0.000000000000000000 ) ) ;
#423 = PLANE ( 'NONE',  #11407 ) ;
#424 = CARTESIAN_POINT ( 'NONE',  ( 0.000000000000000000, -4.857225732735059864E-14, 6.500000000000037303 ) ) ;
#425 = VERTEX_POINT ( 'NONE', #6170 ) ;
#426 = DIRECTION ( 'NONE',  ( -0.000000000000000000, -0.000000000000000000, -1.000000000000000000 ) ) ;
#427 = CARTESIAN_POINT ( 'NONE',  ( -68.99615306438070661, 136.4836397816626743, -167.1454815528550739 ) ) ;
#428 = CARTESIAN_POINT ( 'NONE',  ( -57.08002265617300708, 84.22855780814606419, -167.1454815528550739 ) ) ;
#429 = ORIENTED_EDGE ( 'NONE', *, *, #6145, .F. ) ;
#430 = VECTOR ( 'NONE', #5454, 1000.000000000000000 ) ;
#431 = CARTESIAN_POINT ( 'NONE',  ( -67.77554565888843285, 85.77305660501664875, 15.00000000000006928 ) ) ;
#432 = VECTOR ( 'NONE', #18327, 1000.000000000000000 ) ;
#433 = CARTESIAN_POINT ( 'NONE',  ( 15.23320273812466574, -111.0842361345572158, 57.00000000000000000 ) ) ;
#434 = CIRCLE ( 'NONE', #4026, 12.50000000000001066 ) ;
#435 = ORIENTED_EDGE ( 'NONE', *, *, #15098, .T. ) ;
#436 = VECTOR ( 'NONE', #9546, 1000.000000000000000 ) ;
#437 = ORIENTED_EDGE ( 'NONE', *, *, #1963, .T. ) ;
#438 = ORIENTED_EDGE ( 'NONE', *, *, #10980, .F. ) ;
#439 = CARTESIAN_POINT ( 'NONE',  ( -63.80603561266293156, 73.69239390902558284, -167.1454815528550739 ) ) ;
#440 = EDGE_CURVE ( 'NONE', #16158, #9400, #4619, .T. ) ;
#441 = DIRECTION ( 'NONE',  ( 0.000000000000000000, 0.000000000000000000, 1.000000000000000000 ) ) ;
#442 = LINE ( 'NONE', #4723, #8228 ) ;
#443 =( LENGTH_UNIT ( ) NAMED_UNIT ( * ) SI_UNIT ( .MILLI., .METRE. ) );
#444 = PLANE ( 'NONE',  #8468 ) ;
#445 = DIRECTION ( 'NONE',  ( 0.000000000000000000, 0.000000000000000000, 1.000000000000000000 ) ) ;
#446 = ORIENTED_EDGE ( 'NONE', *, *, #6478, .T. ) ;
#447 = CIRCLE ( 'NONE', #16265, 4.599999999999999645 ) ;
#448 = CARTESIAN_POINT ( 'NONE',  ( -71.24615306438118978, 0.5762228045637974860, -15.00000000000001421 ) ) ;
#449 = CIRCLE ( 'NONE', #2236, 21.04359719766049608 ) ;
#450 = FACE_OUTER_BOUND ( 'NONE', #16283, .T. ) ;
#451 = DIRECTION ( 'NONE',  ( 0.000000000000000000, -5.551115123125748189E-17, -1.000000000000000000 ) ) ;
#452 = AXIS2_PLACEMENT_3D ( 'NONE', #2320, #3822, #12451 ) ;
#453 = CARTESIAN_POINT ( 'NONE',  ( 4.699999999999995737, 5.629165124598635828, -3.250000000000016875 ) ) ;
#454 = DIRECTION ( 'NONE',  ( 0.000000000000000000, 0.000000000000000000, -1.000000000000000000 ) ) ;
#455 = VERTEX_POINT ( 'NONE', #1621 ) ;
#456 = DIRECTION ( 'NONE',  ( 0.000000000000000000, 0.000000000000000000, 1.000000000000000000 ) ) ;
#457 = EDGE_CURVE ( 'NONE', #3111, #2581, #12721, .T. ) ;
#458 = ORIENTED_EDGE ( 'NONE', *, *, #15095, .T. ) ;
#459 = EDGE_CURVE ( 'NONE', #18478, #6989, #7332, .T. ) ;
#460 = DIRECTION ( 'NONE',  ( -0.000000000000000000, -1.000000000000000000, -0.000000000000000000 ) ) ;
#461 = CARTESIAN_POINT ( 'NONE',  ( -36.29822661857599542, 80.88798785482900655, 55.76710478718474917 ) ) ;
#462 = ORIENTED_EDGE ( 'NONE', *, *, #9043, .F. ) ;
#463 = ORIENTED_EDGE ( 'NONE', *, *, #6166, .F. ) ;
#464 = VECTOR ( 'NONE', #12334, 1000.000000000000000 ) ;
#465 = AXIS2_PLACEMENT_3D ( 'NONE', #15310, #8209, #13925 ) ;
#466 = EDGE_CURVE ( 'NONE', #2633, #113, #1358, .T. ) ;
#467 = ORIENTED_EDGE ( 'NONE', *, *, #4024, .T. ) ;
#468 = EDGE_CURVE ( 'NONE', #18251, #15291, #12961, .T. ) ;
#469 = EDGE_CURVE ( 'NONE', #3406, #8935, #14485, .T. ) ;
#470 = CARTESIAN_POINT ( 'NONE',  ( -73.32517902883354566, 66.64375664990241432, 102.5000000000000000 ) ) ;
#471 = CARTESIAN_POINT ( 'NONE',  ( -71.24615306438091977, 72.83285375456371469, 15.00000000000006928 ) ) ;
#472 = DIRECTION ( 'NONE',  ( 1.000000000000000000, 0.000000000000000000, 0.000000000000000000 ) ) ;
#473 = DIRECTION ( 'NONE',  ( 0.3420201433256686574, -0.9396926207859084279, 0.000000000000000000 ) ) ;
#474 = PLANE ( 'NONE',  #12259 ) ;
#475 = DIRECTION ( 'NONE',  ( 1.156482317317869999E-16, 0.000000000000000000, 1.000000000000000000 ) ) ;
#476 = DIRECTION ( 'NONE',  ( 0.000000000000000000, 0.000000000000000000, -1.000000000000000000 ) ) ;
#477 = ORIENTED_EDGE ( 'NONE', *, *, #4383, .F. ) ;
#478 = EDGE_CURVE ( 'NONE', #12432, #2231, #13393, .T. ) ;
#479 = CARTESIAN_POINT ( 'NONE',  ( 0.5805565836007609004, 3.752776749732559924, -6.500000000000061284 ) ) ;
#480 = CARTESIAN_POINT ( 'NONE',  ( -76.37409655828265898, -111.0842361345572158, -2.461913000519969422E-13 ) ) ;
#481 = CARTESIAN_POINT ( 'NONE',  ( 113.3630170098442989, -111.0842361345572158, -3.000000000000000000 ) ) ;
#482 = ORIENTED_EDGE ( 'NONE', *, *, #4046, .F. ) ;
#483 = DIRECTION ( 'NONE',  ( -1.000000000000000000, 0.000000000000000000, -5.022391976381918634E-16 ) ) ;
#484 = DIRECTION ( 'NONE',  ( 0.000000000000000000, 0.000000000000000000, -1.000000000000000000 ) ) ;
#485 = EDGE_CURVE ( 'NONE', #2052, #18444, #13583, .T. ) ;
#486 = ORIENTED_EDGE ( 'NONE', *, *, #1405, .F. ) ;
#487 = ADVANCED_FACE ( 'NONE', ( #16560 ), #14878, .T. ) ;
#488 = ORIENTED_EDGE ( 'NONE', *, *, #10760, .T. ) ;
#489 = EDGE_CURVE ( 'NONE', #6937, #4200, #6985, .T. ) ;
#490 = CARTESIAN_POINT ( 'NONE',  ( -68.99615306438077766, 111.3508985816626335, -167.1454815528550739 ) ) ;
#491 = CARTESIAN_POINT ( 'NONE',  ( -38.40665361001209988, 55.34834135440265612, -23.54080219878014546 ) ) ;
#492 = CARTESIAN_POINT ( 'NONE',  ( -102.4618227840623774, -151.5628872026273086, 57.00000000000000000 ) ) ;
#493 = ORIENTED_EDGE ( 'NONE', *, *, #10731, .F. ) ;
#494 = LINE ( 'NONE', #576, #5416 ) ;
#495 = ORIENTED_EDGE ( 'NONE', *, *, #6626, .T. ) ;
#496 = CARTESIAN_POINT ( 'NONE',  ( 276.3098885457529832, -32.62665103886256190, 7.000000000000010658 ) ) ;
#497 = DIRECTION ( 'NONE',  ( -1.000000000000000000, 0.000000000000000000, 0.000000000000000000 ) ) ;
#498 = CARTESIAN_POINT ( 'NONE',  ( -57.08002265617300708, 84.22855780814606419, -15.00000000000001421 ) ) ;
#499 = CARTESIAN_POINT ( 'NONE',  ( -71.24615306438114715, 10.00100075456375492, -167.1454815528550739 ) ) ;
#500 = ORIENTED_EDGE ( 'NONE', *, *, #3536, .F. ) ;
#501 = ORIENTED_EDGE ( 'NONE', *, *, #3133, .T. ) ;
#502 = FACE_OUTER_BOUND ( 'NONE', #5462, .T. ) ;
#503 = ORIENTED_EDGE ( 'NONE', *, *, #14484, .F. ) ;
#504 = ORIENTED_EDGE ( 'NONE', *, *, #2706, .T. ) ;
#505 = VERTEX_POINT ( 'NONE', #2158 ) ;
#506 = LINE ( 'NONE', #10147, #14475 ) ;
#507 = DIRECTION ( 'NONE',  ( 0.000000000000000000, 0.000000000000000000, 1.000000000000000000 ) ) ;
#508 = ORIENTED_EDGE ( 'NONE', *, *, #8600, .F. ) ;
#509 = LINE ( 'NONE', #239, #10786 ) ;
#510 = DIRECTION ( 'NONE',  ( -0.000000000000000000, 0.000000000000000000, 1.000000000000000000 ) ) ;
#511 = ORIENTED_EDGE ( 'NONE', *, *, #14433, .F. ) ;
#512 = DIRECTION ( 'NONE',  ( 0.000000000000000000, 0.000000000000000000, 1.000000000000000000 ) ) ;
#513 = VERTEX_POINT ( 'NONE', #15067 ) ;
#514 = CARTESIAN_POINT ( 'NONE',  ( -57.08002265617300708, 84.22855780814606419, 15.00000000000006928 ) ) ;
#515 = DIRECTION ( 'NONE',  ( -0.9396926207859008784, 0.3420201433256891965, 0.000000000000000000 ) ) ;
#516 = ORIENTED_EDGE ( 'NONE', *, *, #6768, .F. ) ;
#517 = DIRECTION ( 'NONE',  ( -1.000000000000000000, -3.016910393003147592E-15, 0.000000000000000000 ) ) ;
#518 = DIRECTION ( 'NONE',  ( 1.000000000000000000, 0.000000000000000000, 0.000000000000000000 ) ) ;
#519 = ORIENTED_EDGE ( 'NONE', *, *, #11473, .F. ) ;
#520 = ORIENTED_EDGE ( 'NONE', *, *, #4378, .T. ) ;
#521 = ORIENTED_EDGE ( 'NONE', *, *, #1743, .F. ) ;
#522 = DIRECTION ( 'NONE',  ( 0.000000000000000000, 0.000000000000000000, 1.000000000000000000 ) ) ;
#523 = EDGE_LOOP ( 'NONE', ( #7059, #9577, #8331, #14594 ) ) ;
#524 = APPLICATION_PROTOCOL_DEFINITION ( 'draft international standard', 'automotive_design', 1998, #2022 ) ;
#525 = CYLINDRICAL_SURFACE ( 'NONE', #10315, 9.999999999999994671 ) ;
#526 = DIRECTION ( 'NONE',  ( 0.000000000000000000, 0.000000000000000000, 1.000000000000000000 ) ) ;
#527 = CARTESIAN_POINT ( 'NONE',  ( -68.99615306438094819, 54.80223088166269463, 15.00000000000006928 ) ) ;
#528 = EDGE_LOOP ( 'NONE', ( #8354, #7996, #14007, #17143 ) ) ;
#529 = CARTESIAN_POINT ( 'NONE',  ( -68.99615306438074924, 121.3905323881302962, -167.1454815528550739 ) ) ;
#530 = CARTESIAN_POINT ( 'NONE',  ( -66.63376473465912397, -19.34983604512935429, 57.00000000000000000 ) ) ;
#531 = CARTESIAN_POINT ( 'NONE',  ( -71.24615306438101925, 31.99214930456378880, 15.00000000000006928 ) ) ;
#532 = CARTESIAN_POINT ( 'NONE',  ( -67.59262256747319952, 110.5691553257988460, -30.35917033480640370 ) ) ;
#533 = VECTOR ( 'NONE', #2270, 1000.000000000000000 ) ;
#534 = CARTESIAN_POINT ( 'NONE',  ( -36.04074381574865527, 84.72093613475881568, 69.98790959730909833 ) ) ;
#535 = VERTEX_POINT ( 'NONE', #769 ) ;
#536 = LINE ( 'NONE', #14927, #15963 ) ;
#537 = DIRECTION ( 'NONE',  ( 0.000000000000000000, 1.000000000000000000, 0.000000000000000000 ) ) ;
#538 = VERTEX_POINT ( 'NONE', #3755 ) ;
#539 = EDGE_CURVE ( 'NONE', #1636, #14316, #3687, .T. ) ;
#540 = CARTESIAN_POINT ( 'NONE',  ( -107.5926225674731711, 57.88796029049330372, -26.35917033480641436 ) ) ;
#541 = DIRECTION ( 'NONE',  ( -1.000000000000000000, 0.000000000000000000, 0.000000000000000000 ) ) ;
#542 = ORIENTED_EDGE ( 'NONE', *, *, #17582, .T. ) ;
#543 = ORIENTED_EDGE ( 'NONE', *, *, #11265, .T. ) ;
#544 = AXIS2_PLACEMENT_3D ( 'NONE', #10480, #10583, #14958 ) ;
#545 = ORIENTED_EDGE ( 'NONE', *, *, #18144, .T. ) ;
#546 = DIRECTION ( 'NONE',  ( 1.000000000000000000, 0.000000000000000000, 0.000000000000000000 ) ) ;
#547 = CARTESIAN_POINT ( 'NONE',  ( -71.24615306438089135, 81.36876096522922808, 15.00000000000006928 ) ) ;
#548 = EDGE_CURVE ( 'NONE', #15230, #8556, #6062, .T. ) ;
#549 = FACE_OUTER_BOUND ( 'NONE', #11506, .T. ) ;
#550 = CARTESIAN_POINT ( 'NONE',  ( 124.5381772159375942, -151.5628872026272802, 57.00000000000000000 ) ) ;
#551 = CARTESIAN_POINT ( 'NONE',  ( -57.08002265617301418, 106.1506877598988154, 97.49999999999998579 ) ) ;
#552 = CARTESIAN_POINT ( 'NONE',  ( -86.44887054343442401, 84.22855780814606419, -15.00000000000000711 ) ) ;
#553 = PRODUCT_DEFINITION_SHAPE ( 'NONE', 'NONE',  #18520 ) ;
#554 = ORIENTED_EDGE ( 'NONE', *, *, #15682, .F. ) ;
#555 = LINE ( 'NONE', #16078, #14389 ) ;
#556 = CARTESIAN_POINT ( 'NONE',  ( -76.09645744896180020, 61.84763831329342310, -26.96898856272271772 ) ) ;
#557 = DIRECTION ( 'NONE',  ( -0.9396926207859093161, 0.3420201433256661594, 0.000000000000000000 ) ) ;
#558 = VECTOR ( 'NONE', #1688, 1000.000000000000000 ) ;
#559 = ORIENTED_EDGE ( 'NONE', *, *, #11791, .T. ) ;
#560 = EDGE_CURVE ( 'NONE', #11029, #18478, #7961, .T. ) ;
#561 = ADVANCED_FACE ( 'NONE', ( #13672, #6655 ), #7775, .T. ) ;
#562 = DIRECTION ( 'NONE',  ( 0.000000000000000000, 0.000000000000000000, 1.000000000000000000 ) ) ;
#563 = DIRECTION ( 'NONE',  ( 0.000000000000000000, 0.000000000000000000, 1.000000000000000000 ) ) ;
#564 = ORIENTED_EDGE ( 'NONE', *, *, #8838, .T. ) ;
#565 = VERTEX_POINT ( 'NONE', #10486 ) ;
#566 = ADVANCED_FACE ( 'NONE', ( #8045 ), #954, .T. ) ;
#567 = DIRECTION ( 'NONE',  ( 1.000000000000000000, 0.000000000000000000, 5.077734830647299712E-16 ) ) ;
#568 = DIRECTION ( 'NONE',  ( 0.3420201433256649937, -0.9396926207859097602, 0.000000000000000000 ) ) ;
#570 = ADVANCED_FACE ( 'NONE', ( #7868 ), #12377, .F. ) ;
#569 = TOROIDAL_SURFACE ( 'NONE', #11925, 10.04359719766049963, 1.000000000000000000 ) ;
#571 = DIRECTION ( 'NONE',  ( 1.000000000000000000, 0.000000000000000000, 0.000000000000000000 ) ) ;
#572 = DIRECTION ( 'NONE',  ( -5.204170427930409450E-16, 0.000000000000000000, 1.000000000000000000 ) ) ;
#573 = VERTEX_POINT ( 'NONE', #14965 ) ;
#574 = CARTESIAN_POINT ( 'NONE',  ( -71.24615306438076345, 132.5231141045637457, -15.00000000000001421 ) ) ;
#575 = VECTOR ( 'NONE', #9890, 1000.000000000000000 ) ;
#576 = CARTESIAN_POINT ( 'NONE',  ( -71.24615306438084872, 72.83285375456374311, 15.00000000000006928 ) ) ;
#577 = EDGE_CURVE ( 'NONE', #10391, #5674, #7997, .T. ) ;
#578 = ORIENTED_EDGE ( 'NONE', *, *, #6429, .T. ) ;
#579 = CARTESIAN_POINT ( 'NONE',  ( -69.52933024547458274, 85.35316464920589397, -15.00000000000001421 ) ) ;
#580 = FACE_OUTER_BOUND ( 'NONE', #1981, .T. ) ;
#581 = DIRECTION ( 'NONE',  ( -0.9396926207859084279, 0.3420201433256686574, 1.086737899652989892E-16 ) ) ;
#582 = DIRECTION ( 'NONE',  ( -1.000000000000000000, 0.000000000000000000, -6.950654929607132427E-15 ) ) ;
#583 = VERTEX_POINT ( 'NONE', #16183 ) ;
#584 = CARTESIAN_POINT ( 'NONE',  ( -71.24615306438091977, 71.94398301522919326, 15.00000000000006928 ) ) ;
#585 = ORIENTED_EDGE ( 'NONE', *, *, #478, .F. ) ;
#586 = EDGE_CURVE ( 'NONE', #15423, #5470, #3374, .T. ) ;
#587 = EDGE_CURVE ( 'NONE', #1317, #10161, #1984, .T. ) ;
#588 = CARTESIAN_POINT ( 'NONE',  ( -127.5926225674731711, 57.88796029049329661, -22.35917033480642502 ) ) ;
#589 = ORIENTED_EDGE ( 'NONE', *, *, #5376, .F. ) ;
#590 = VECTOR ( 'NONE', #9664, 1000.000000000000000 ) ;
#591 = ORIENTED_EDGE ( 'NONE', *, *, #12155, .F. ) ;
#592 = CIRCLE ( 'NONE', #14907, 7.168074330098680669 ) ;
#593 = VERTEX_POINT ( 'NONE', #12274 ) ;
#594 = CARTESIAN_POINT ( 'NONE',  ( -68.99615306438083451, 95.64293533166268446, -167.1454815528550739 ) ) ;
#595 = CARTESIAN_POINT ( 'NONE',  ( -78.12361985383350316, 84.22855780814606419, 77.50000000000000000 ) ) ;
#596 = DIRECTION ( 'NONE',  ( -0.9396926207859171987, 0.3420201433256445100, -4.890320548438495251E-16 ) ) ;
#597 = ORIENTED_EDGE ( 'NONE', *, *, #9244, .F. ) ;
#598 = DIRECTION ( 'NONE',  ( 0.000000000000000000, 0.000000000000000000, 1.000000000000000000 ) ) ;
#599 = VECTOR ( 'NONE', #9080, 1000.000000000000000 ) ;
#600 = EDGE_CURVE ( 'NONE', #16048, #10561, #5150, .T. ) ;
#601 = DIRECTION ( 'NONE',  ( 1.156482317317869999E-16, 0.000000000000000000, 1.000000000000000000 ) ) ;
#602 = ORIENTED_EDGE ( 'NONE', *, *, #17269, .T. ) ;
#603 = PLANE ( 'NONE',  #8410 ) ;
#604 = AXIS2_PLACEMENT_3D ( 'NONE', #7949, #3633, #837 ) ;
#605 = ORIENTED_EDGE ( 'NONE', *, *, #15039, .T. ) ;
#606 = AXIS2_PLACEMENT_3D ( 'NONE', #17023, #8618, #18357 ) ;
#607 = FACE_OUTER_BOUND ( 'NONE', #6469, .T. ) ;
#608 = CARTESIAN_POINT ( 'NONE',  ( -66.46434123065944277, 108.9297695310272331, 25.00000000000000000 ) ) ;
#609 = ORIENTED_EDGE ( 'NONE', *, *, #8356, .T. ) ;
#610 = B_SPLINE_CURVE_WITH_KNOTS ( 'NONE', 3,
 ( #15647, #8545, #1426, #14249, #5805, #17565, #12326, #377, #10719, #3183, #10817, #4747, #15119, #3714, #16415, #3604, #897, #9324, #15203, #10926, #9506, #8984, #5202, #15020, #6601, #11795, #10297, #18019, #2389, #3804, #8096, #8894, #16611, #14677, #12219, #2299, #13815, #1004, #2211, #8002, #12429, #6705, #16072, #13198, #6066, #16515 ),
 .UNSPECIFIED., .F., .F.,
 ( 4, 2, 2, 2, 2, 2, 2, 2, 2, 2, 2, 2, 2, 2, 2, 2, 2, 2, 2, 2, 2, 2, 4 ),
 ( 1.387778780781445676E-17, 0.001477780233738794748, 0.002216670350608189195, 0.002955560467477583424, 0.004433340701216313337, 0.005172230818085679811, 0.005911120934955047153, 0.007388901168693846888, 0.008866681402432645756, 0.009605571519302056466, 0.01034446163617146891, 0.01182224186991029206, 0.01330002210364911869, 0.01477780233738794531, 0.01625558257112677193, 0.01699447268799620173, 0.01773336280486562805, 0.01921114303860447722, 0.01995003315547392089, 0.02068892327234336456, 0.02216670350608221027, 0.02290559362295161577, 0.02364448373982101781 ),
 .UNSPECIFIED. ) ;
#611 = CARTESIAN_POINT ( 'NONE',  ( -67.59262256747319952, 110.5691553257988460, 26.35917033480641436 ) ) ;
#612 = VECTOR ( 'NONE', #541, 1000.000000000000000 ) ;
#613 = DIRECTION ( 'NONE',  ( 0.000000000000000000, 0.000000000000000000, 1.000000000000000000 ) ) ;
#614 = ORIENTED_EDGE ( 'NONE', *, *, #15108, .F. ) ;
#615 = AXIS2_PLACEMENT_3D ( 'NONE', #18506, #12902, #11404 ) ;
#616 = VERTEX_POINT ( 'NONE', #17966 ) ;
#617 = VECTOR ( 'NONE', #5671, 1000.000000000000000 ) ;
#618 = EDGE_LOOP ( 'NONE', ( #14564, #14000, #6336, #1242 ) ) ;
#619 = LINE ( 'NONE', #17908, #9368 ) ;
#620 = CYLINDRICAL_SURFACE ( 'NONE', #5187, 5.654315315325682434 ) ;
#621 = ORIENTED_EDGE ( 'NONE', *, *, #9768, .T. ) ;
#622 = APPLICATION_PROTOCOL_DEFINITION ( 'draft international standard', 'automotive_design', 1998, #9441 ) ;
#623 = DIRECTION ( 'NONE',  ( 1.000000000000000000, 2.062304371594500740E-16, 0.000000000000000000 ) ) ;
#624 = CARTESIAN_POINT ( 'NONE',  ( -66.02736529514692165, 75.49957964911740760, -167.1454815528550739 ) ) ;
#625 = CARTESIAN_POINT ( 'NONE',  ( -68.99615306438089135, 79.93497208166267853, -167.1454815528550739 ) ) ;
#626 = VERTEX_POINT ( 'NONE', #9934 ) ;
#627 = CIRCLE ( 'NONE', #12604, 47.49926016644946714 ) ;
#628 = CARTESIAN_POINT ( 'NONE',  ( -71.24615306438089135, 84.51035361522924916, -167.1454815528550739 ) ) ;
#629 = DIRECTION ( 'NONE',  ( 0.3420201433256649937, -0.9396926207859097602, 0.000000000000000000 ) ) ;
#630 = DIRECTION ( 'NONE',  ( 0.000000000000000000, 0.000000000000000000, 1.000000000000000000 ) ) ;
#631 = DIRECTION ( 'NONE',  ( 0.000000000000000000, 0.000000000000000000, 1.000000000000000000 ) ) ;
#632 = CARTESIAN_POINT ( 'NONE',  ( 15.23320273812466041, -46.83756720124470263, -57.00000000000000000 ) ) ;
#633 = ORIENTED_EDGE ( 'NONE', *, *, #7187, .F. ) ;
#634 = AXIS2_PLACEMENT_3D ( 'NONE', #7986, #512, #13420 ) ;
#635 = VECTOR ( 'NONE', #5666, 1000.000000000000000 ) ;
#636 = CARTESIAN_POINT ( 'NONE',  ( -71.24615306438086293, 90.79353891522923448, 15.00000000000006928 ) ) ;
#637 = DIRECTION ( 'NONE',  ( -1.000000000000000000, -0.000000000000000000, -0.000000000000000000 ) ) ;
#638 = ORIENTED_EDGE ( 'NONE', *, *, #9, .F. ) ;
#639 = DIRECTION ( 'NONE',  ( 0.000000000000000000, 1.000000000000000000, 0.000000000000000000 ) ) ;
#640 = CARTESIAN_POINT ( 'NONE',  ( -42.53669312409158465, -96.08423613455721579, 5.204170427930421283E-15 ) ) ;
#641 = EDGE_LOOP ( 'NONE', ( #13099, #15798 ) ) ;
#642 = EDGE_CURVE ( 'NONE', #11067, #11836, #18161, .T. ) ;
#643 = ORIENTED_EDGE ( 'NONE', *, *, #17487, .T. ) ;
#644 = AXIS2_PLACEMENT_3D ( 'NONE', #13035, #12849, #9845 ) ;
#645 = LINE ( 'NONE', #6439, #5474 ) ;
#646 = VERTEX_POINT ( 'NONE', #12557 ) ;
#647 = AXIS2_PLACEMENT_3D ( 'NONE', #8443, #1344, #3846 ) ;
#648 = DIRECTION ( 'NONE',  ( -5.204170427930409450E-16, 0.000000000000000000, 1.000000000000000000 ) ) ;
#649 = DIRECTION ( 'NONE',  ( 0.000000000000000000, 0.000000000000000000, 1.000000000000000000 ) ) ;
#650 = DIRECTION ( 'NONE',  ( 0.000000000000000000, 0.000000000000000000, -1.000000000000000000 ) ) ;
#651 = PLANE ( 'NONE',  #16727 ) ;
#652 = LINE ( 'NONE', #7583, #6407 ) ;
#653 = LINE ( 'NONE', #5038, #16770 ) ;
#654 = ORIENTED_EDGE ( 'NONE', *, *, #15337, .F. ) ;
#655 = AXIS2_PLACEMENT_3D ( 'NONE', #13524, #709, #7704 ) ;
#656 = CARTESIAN_POINT ( 'NONE',  ( -75.85991620623855169, 61.64845565236244340, -24.98030658468874066 ) ) ;
#657 = DIRECTION ( 'NONE',  ( 0.9396926207859097602, 0.3420201433256649937, -1.086737899652991371E-16 ) ) ;
#658 = ORIENTED_EDGE ( 'NONE', *, *, #15578, .F. ) ;
#659 = AXIS2_PLACEMENT_3D ( 'NONE', #1736, #329, #11753 ) ;
#660 = CARTESIAN_POINT ( 'NONE',  ( -98.90286936182226896, -91.08423613455721579, -10.65431531532588316 ) ) ;
#661 = AXIS2_PLACEMENT_3D ( 'NONE', #357, #3872, #9580 ) ;
#662 = CARTESIAN_POINT ( 'NONE',  ( -76.37409655828280108, -111.0842361345572158, 45.05044770573179846 ) ) ;
#663 = VERTEX_POINT ( 'NONE', #5536 ) ;
#664 = ORIENTED_EDGE ( 'NONE', *, *, #16224, .F. ) ;
#665 = UNCERTAINTY_MEASURE_WITH_UNIT (LENGTH_MEASURE( 1.000000000000000082E-05 ), #5405, 'distance_accuracy_value', 'NONE');
#666 = AXIS2_PLACEMENT_3D ( 'NONE', #5456, #2751, #8462 ) ;
#667 = CARTESIAN_POINT ( 'NONE',  ( -66.96222586426215173, 88.60139997190893268, -15.00000000000001421 ) ) ;
#668 = LINE ( 'NONE', #15256, #2163 ) ;
#669 = CARTESIAN_POINT ( 'NONE',  ( -67.26033723204500347, 83.04399200740374454, -167.1454815528550739 ) ) ;
#670 = DIRECTION ( 'NONE',  ( -0.000000000000000000, 1.000000000000000000, -0.000000000000000000 ) ) ;
#671 = ORIENTED_EDGE ( 'NONE', *, *, #12194, .T. ) ;
#672 = ADVANCED_FACE ( 'NONE', ( #7128 ), #8252, .T. ) ;
#673 = CIRCLE ( 'NONE', #13222, 4.599999999999992539 ) ;
#674 = CARTESIAN_POINT ( 'NONE',  ( -76.06514409945376087, 73.26749283226919829, 97.49999999999998579 ) ) ;
#675 = VECTOR ( 'NONE', #2082, 1000.000000000000000 ) ;
#676 = DIRECTION ( 'NONE',  ( -2.062304371594500740E-16, 1.000000000000000000, 0.000000000000000000 ) ) ;
#677 = VERTEX_POINT ( 'NONE', #15453 ) ;
#678 = EDGE_CURVE ( 'NONE', #17304, #14302, #10606, .T. ) ;
#679 = CYLINDRICAL_SURFACE ( 'NONE', #15266, 180.8515291679561585 ) ;
#680 = DIRECTION ( 'NONE',  ( 1.000000000000000000, 2.062304371594500494E-16, -0.000000000000000000 ) ) ;
#681 = CARTESIAN_POINT ( 'NONE',  ( -208.2552686774341737, 84.22855780814606419, 55.12736457073573604 ) ) ;
#682 = CYLINDRICAL_SURFACE ( 'NONE', #6960, 3.999999999999996447 ) ;
#683 = ORIENTED_EDGE ( 'NONE', *, *, #10429, .F. ) ;
#684 = FACE_OUTER_BOUND ( 'NONE', #230, .T. ) ;
#685 = ORIENTED_EDGE ( 'NONE', *, *, #12458, .T. ) ;
#686 = VECTOR ( 'NONE', #9007, 1000.000000000000000 ) ;
#687 = EDGE_CURVE ( 'NONE', #18482, #6976, #11196, .T. ) ;
#688 = LINE ( 'NONE', #4887, #17550 ) ;
#689 = VERTEX_POINT ( 'NONE', #6938 ) ;
#690 = ADVANCED_FACE ( 'NONE', ( #9649 ), #1237, .F. ) ;
#691 = ADVANCED_FACE ( 'NONE', ( #15360 ), #11052, .T. ) ;
#692 = VECTOR ( 'NONE', #1319, 1000.000000000000000 ) ;
#693 = AXIS2_PLACEMENT_3D ( 'NONE', #2208, #12136, #2384 ) ;
#694 = ORIENTED_EDGE ( 'NONE', *, *, #12829, .T. ) ;
#695 = FACE_OUTER_BOUND ( 'NONE', #12047, .T. ) ;
#696 = CARTESIAN_POINT ( 'NONE',  ( -42.53669312409158465, -96.08423613455721579, 5.204170427930421283E-15 ) ) ;
#697 = ADVANCED_FACE ( 'NONE', ( #8543 ), #8438, .T. ) ;
#698 = ORIENTED_EDGE ( 'NONE', *, *, #15200, .T. ) ;
#699 = EDGE_CURVE ( 'NONE', #12065, #18179, #4050, .T. ) ;
#700 = EDGE_CURVE ( 'NONE', #5246, #2130, #14481, .T. ) ;
#701 = DIRECTION ( 'NONE',  ( -0.000000000000000000, -1.000000000000000000, -0.000000000000000000 ) ) ;
#702 = DIRECTION ( 'NONE',  ( 0.9396926207859097602, 0.3420201433256649381, 4.890320548438455808E-16 ) ) ;
#703 = VERTEX_POINT ( 'NONE', #18363 ) ;
#704 = EDGE_CURVE ( 'NONE', #3211, #1616, #14247, .T. ) ;
#705 = DIRECTION ( 'NONE',  ( 0.000000000000000000, 0.000000000000000000, 1.000000000000000000 ) ) ;
#706 = VECTOR ( 'NONE', #17635, 1000.000000000000000 ) ;
#707 = ORIENTED_EDGE ( 'NONE', *, *, #4942, .F. ) ;
#708 = CIRCLE ( 'NONE', #7867, 10.24899999999999345 ) ;
#709 = DIRECTION ( 'NONE',  ( 0.000000000000000000, -0.000000000000000000, -1.000000000000000000 ) ) ;
#710 = DIRECTION ( 'NONE',  ( -1.000000000000000000, 0.000000000000000000, 1.692578276882434470E-16 ) ) ;
#711 = ORIENTED_EDGE ( 'NONE', *, *, #17825, .T. ) ;
#712 = ADVANCED_FACE ( 'NONE', ( #1423 ), #18070, .F. ) ;
#713 = CARTESIAN_POINT ( 'NONE',  ( 49.38736944425944841, -141.5628872026273086, -57.00000000000000000 ) ) ;
#714 = LINE ( 'NONE', #6406, #14338 ) ;
#715 = VERTEX_POINT ( 'NONE', #12761 ) ;
#716 = EDGE_CURVE ( 'NONE', #3636, #2613, #10963, .T. ) ;
#717 = EDGE_CURVE ( 'NONE', #13256, #9250, #2635, .T. ) ;
#718 = DIRECTION ( 'NONE',  ( -1.000000000000000000, 0.000000000000000000, 0.000000000000000000 ) ) ;
#719 = AXIS2_PLACEMENT_3D ( 'NONE', #3606, #2301, #18126 ) ;
#720 = AXIS2_PLACEMENT_3D ( 'NONE', #17412, #15835, #3025 ) ;
#721 = ORIENTED_EDGE ( 'NONE', *, *, #229, .F. ) ;
#722 = DIRECTION ( 'NONE',  ( 0.9396926207859185309, 0.3420201433256406798, -1.086737899653001478E-16 ) ) ;
#723 = LINE ( 'NONE', #6211, #4284 ) ;
#724 = ORIENTED_EDGE ( 'NONE', *, *, #2535, .T. ) ;
#725 = FACE_OUTER_BOUND ( 'NONE', #5235, .T. ) ;
#726 = CARTESIAN_POINT ( 'NONE',  ( 5.233202738124663966, -15.18076580469977621, 54.12731639097741976 ) ) ;
#727 = EDGE_CURVE ( 'NONE', #299, #9555, #15255, .T. ) ;
#728 = CYLINDRICAL_SURFACE ( 'NONE', #10885, 4.600000000000006750 ) ;
#729 = ORIENTED_EDGE ( 'NONE', *, *, #18046, .T. ) ;
#730 = PRESENTATION_LAYER_ASSIGNMENT (  '', '', ( #9101 ) ) ;
#731 = CARTESIAN_POINT ( 'NONE',  ( -68.99615306438083451, 101.9261206316626698, -15.00000000000001421 ) ) ;
#732 = DIRECTION ( 'NONE',  ( 0.000000000000000000, 0.000000000000000000, -1.000000000000000000 ) ) ;
#733 = FACE_OUTER_BOUND ( 'NONE', #14539, .T. ) ;
#734 = DIRECTION ( 'NONE',  ( -1.000000000000000000, -0.000000000000000000, -0.000000000000000000 ) ) ;
#735 = ORIENTED_EDGE ( 'NONE', *, *, #7900, .T. ) ;
#736 = VECTOR ( 'NONE', #16621, 1000.000000000000000 ) ;
#737 = VECTOR ( 'NONE', #7847, 1000.000000000000000 ) ;
#738 = LINE ( 'NONE', #6614, #17449 ) ;
#739 = CARTESIAN_POINT ( 'NONE',  ( -127.5926225674731711, 57.88796029049329661, 26.35917033480641436 ) ) ;
#740 = ORIENTED_EDGE ( 'NONE', *, *, #13031, .T. ) ;
#741 = PLANE ( 'NONE',  #2390 ) ;
#742 = CARTESIAN_POINT ( 'NONE',  ( -36.67168494155210112, 79.09395985567564935, 57.02782509738743499 ) ) ;
#743 = ORIENTED_EDGE ( 'NONE', *, *, #17825, .F. ) ;
#744 = EDGE_LOOP ( 'NONE', ( #10644, #10859, #13993, #8792 ) ) ;
#745 = TOROIDAL_SURFACE ( 'NONE', #11214, 40.40389983439752086, 5.000000000000000000 ) ;
#746 = DIRECTION ( 'NONE',  ( 0.000000000000000000, 0.000000000000000000, -1.000000000000000000 ) ) ;
#747 = AXIS2_PLACEMENT_3D ( 'NONE', #4168, #2377, #13908 ) ;
#748 = VERTEX_POINT ( 'NONE', #8151 ) ;
#749 = VECTOR ( 'NONE', #11083, 1000.000000000000000 ) ;
#750 = CARTESIAN_POINT ( 'NONE',  ( -71.24615306438106188, 34.24487121522926003, -167.1454815528550739 ) ) ;
#751 = DIRECTION ( 'NONE',  ( -0.9396926207859068736, 0.3420201433256726542, 0.000000000000000000 ) ) ;
#752 = CARTESIAN_POINT ( 'NONE',  ( -66.09157170483439359, 57.23989889526016839, 25.00000000000000711 ) ) ;
#753 = CYLINDRICAL_SURFACE ( 'NONE', #2101, 10.24900000000000055 ) ;
#754 = DIRECTION ( 'NONE',  ( 0.000000000000000000, 0.000000000000000000, 1.000000000000000000 ) ) ;
#755 = CARTESIAN_POINT ( 'NONE',  ( -107.5926225674731711, 57.88796029049330372, 26.35917033480641436 ) ) ;
#756 = ORIENTED_EDGE ( 'NONE', *, *, #11242, .F. ) ;
#757 = EDGE_CURVE ( 'NONE', #8476, #13829, #13867, .T. ) ;
#758 = CARTESIAN_POINT ( 'NONE',  ( -73.90024509548729270, 60.14960425286541579, -23.04802554496307820 ) ) ;
#759 = DIRECTION ( 'NONE',  ( 9.117856171852156377E-15, 0.000000000000000000, 1.000000000000000000 ) ) ;
#760 = ORIENTED_EDGE ( 'NONE', *, *, #9977, .T. ) ;
#761 = AXIS2_PLACEMENT_3D ( 'NONE', #9787, #18401, #5568 ) ;
#762 = EDGE_CURVE ( 'NONE', #13170, #4868, #14675, .T. ) ;
#763 = CARTESIAN_POINT ( 'NONE',  ( -31.57667891805219895, -91.08423613455724421, -10.52509945732311891 ) ) ;
#764 = CIRCLE ( 'NONE', #13025, 4.400000000000027889 ) ;
#765 = CARTESIAN_POINT ( 'NONE',  ( -68.99615306438089135, 79.93497208166267853, -15.00000000000001421 ) ) ;
#767 = EDGE_LOOP ( 'NONE', ( #9960, #18341, #6910, #3598, #2917, #14530, #2645, #13701 ) ) ;
#766 = CIRCLE ( 'NONE', #8554, 4.599999999999992539 ) ;
#768 = VERTEX_POINT ( 'NONE', #8808 ) ;
#769 = CARTESIAN_POINT ( 'NONE',  ( -92.59262256747321373, 117.8748711238780373, -35.00000000000000000 ) ) ;
#770 = CARTESIAN_POINT ( 'NONE',  ( -68.99615306438093398, 55.41708673813027985, -15.00000000000001421 ) ) ;
#771 = DIRECTION ( 'NONE',  ( 0.000000000000000000, 0.000000000000000000, 1.000000000000000000 ) ) ;
#772 = DIRECTION ( 'NONE',  ( 0.000000000000000000, 1.000000000000000000, 0.000000000000000000 ) ) ;
#773 = VERTEX_POINT ( 'NONE', #14509 ) ;
#774 = CARTESIAN_POINT ( 'NONE',  ( -69.56651066787533466, 84.80960611389535586, -15.00000000000001421 ) ) ;
#775 = CARTESIAN_POINT ( 'NONE',  ( -71.24615306438109030, 31.99214930456376038, -167.1454815528550739 ) ) ;
#776 = ORIENTED_EDGE ( 'NONE', *, *, #15222, .T. ) ;
#777 = LINE ( 'NONE', #16857, #3625 ) ;
#778 = DIRECTION ( 'NONE',  ( 0.000000000000000000, 0.000000000000000000, 1.000000000000000000 ) ) ;
#779 = CARTESIAN_POINT ( 'NONE',  ( -76.88569266382195622, 91.34252568597634081, 60.07430202819471532 ) ) ;
#780 = DIRECTION ( 'NONE',  ( -1.000000000000000000, -0.000000000000000000, -0.000000000000000000 ) ) ;
#781 = ORIENTED_EDGE ( 'NONE', *, *, #10127, .F. ) ;
#782 = CARTESIAN_POINT ( 'NONE',  ( -48.13268001719898592, 75.49957964911752129, -15.00000000000001421 ) ) ;
#783 = ORIENTED_EDGE ( 'NONE', *, *, #8501, .F. ) ;
#784 = DIRECTION ( 'NONE',  ( -1.000000000000000000, 0.000000000000000000, -0.000000000000000000 ) ) ;
#785 = ORIENTED_EDGE ( 'NONE', *, *, #3442, .T. ) ;
#786 = EDGE_CURVE ( 'NONE', #3445, #7663, #276, .T. ) ;
#787 = EDGE_LOOP ( 'NONE', ( #8636, #4060, #891, #3393 ) ) ;
#788 = DIRECTION ( 'NONE',  ( 0.000000000000000000, 0.000000000000000000, 1.000000000000000000 ) ) ;
#789 = DIRECTION ( 'NONE',  ( 0.000000000000000000, 0.000000000000000000, 1.000000000000000000 ) ) ;
#790 = ORIENTED_EDGE ( 'NONE', *, *, #9217, .T. ) ;
#791 = CARTESIAN_POINT ( 'NONE',  ( -92.59262256747319952, 57.88796029049329661, -26.35917033480641436 ) ) ;
#792 = EDGE_CURVE ( 'NONE', #14885, #13327, #7392, .T. ) ;
#793 = DIRECTION ( 'NONE',  ( 0.3420201433256686574, 0.9396926207859084279, -0.000000000000000000 ) ) ;
#794 = VERTEX_POINT ( 'NONE', #4665 ) ;
#795 = EDGE_CURVE ( 'NONE', #3445, #14282, #1597, .T. ) ;
#796 = PLANE ( 'NONE',  #1250 ) ;
#797 = VERTEX_POINT ( 'NONE', #1868 ) ;
#798 = DIRECTION ( 'NONE',  ( -0.000000000000000000, -0.000000000000000000, -1.000000000000000000 ) ) ;
#799 = DIRECTION ( 'NONE',  ( 1.000000000000000000, 0.000000000000000000, -0.000000000000000000 ) ) ;
#800 = VERTEX_POINT ( 'NONE', #13028 ) ;
#801 = LINE ( 'NONE', #2012, #10914 ) ;
#802 = ADVANCED_FACE ( 'NONE', ( #10295 ), #10201, .F. ) ;
#803 = EDGE_CURVE ( 'NONE', #10920, #7762, #4578, .T. ) ;
#804 = CARTESIAN_POINT ( 'NONE',  ( -102.4618227840623774, -151.5628872026273086, -36.00000000000000000 ) ) ;
#805 = EDGE_LOOP ( 'NONE', ( #18504, #2083, #17066, #16197 ) ) ;
#806 = ORIENTED_EDGE ( 'NONE', *, *, #924, .F. ) ;
#807 = CARTESIAN_POINT ( 'NONE',  ( -57.08002265617300708, 84.22855780814606419, -35.00000000000000711 ) ) ;
#808 = PLANE ( 'NONE',  #6070 ) ;
#809 = EDGE_CURVE ( 'NONE', #10849, #8377, #8807, .T. ) ;
#810 = ORIENTED_EDGE ( 'NONE', *, *, #7346, .F. ) ;
#811 = PLANE ( 'NONE',  #4935 ) ;
#812 =( NAMED_UNIT ( * ) SI_UNIT ( $, .STERADIAN. ) SOLID_ANGLE_UNIT ( ) );
#813 = LINE ( 'NONE', #6502, #11347 ) ;
#814 = DIRECTION ( 'NONE',  ( -0.9396926207859084279, 0.3420201433256686574, 1.086737899652989892E-16 ) ) ;
#815 = EDGE_CURVE ( 'NONE', #6999, #415, #2223, .T. ) ;
#816 = PLANE ( 'NONE',  #16541 ) ;
#817 = ORIENTED_EDGE ( 'NONE', *, *, #18293, .F. ) ;
#818 = DIRECTION ( 'NONE',  ( 1.000000000000000000, 2.062304371594500494E-16, 0.000000000000000000 ) ) ;
#819 = DIRECTION ( 'NONE',  ( 0.000000000000000000, 0.000000000000000000, -1.000000000000000000 ) ) ;
#820 = EDGE_CURVE ( 'NONE', #14582, #7975, #4478, .T. ) ;
#821 = LINE ( 'NONE', #15125, #1960 ) ;
#822 = EDGE_CURVE ( 'NONE', #1101, #833, #157, .T. ) ;
#823 = CARTESIAN_POINT ( 'NONE',  ( -68.99615306438094819, 64.84186468813030046, -15.00000000000001421 ) ) ;
#824 = ORIENTED_EDGE ( 'NONE', *, *, #14638, .T. ) ;
#825 = DIRECTION ( 'NONE',  ( 0.000000000000000000, 1.000000000000000000, 0.000000000000000000 ) ) ;
#826 = CARTESIAN_POINT ( 'NONE',  ( -68.99615306438080609, 105.6825691381303045, -15.00000000000001421 ) ) ;
#827 = VERTEX_POINT ( 'NONE', #1769 ) ;
#828 = EDGE_CURVE ( 'NONE', #10611, #5567, #16268, .T. ) ;
#829 = DIRECTION ( 'NONE',  ( 0.000000000000000000, 0.000000000000000000, 1.000000000000000000 ) ) ;
#830 = ORIENTED_EDGE ( 'NONE', *, *, #10988, .T. ) ;
#831 = ORIENTED_EDGE ( 'NONE', *, *, #18311, .F. ) ;
#832 = CARTESIAN_POINT ( 'NONE',  ( -63.25151023250651150, 93.09943318379590949, -15.00000000000001421 ) ) ;
#833 = VERTEX_POINT ( 'NONE', #374 ) ;
#834 = CARTESIAN_POINT ( 'NONE',  ( -44.63071506687145984, 85.35316464920607871, 15.00000000000009592 ) ) ;
#835 = DIRECTION ( 'NONE',  ( 0.000000000000000000, 0.000000000000000000, 1.000000000000000000 ) ) ;
#836 = LINE ( 'NONE', #4020, #9670 ) ;
#837 = DIRECTION ( 'NONE',  ( 1.000000000000000000, 0.000000000000000000, 0.000000000000000000 ) ) ;
#838 = CARTESIAN_POINT ( 'NONE',  ( -64.09025127992788384, 50.58224449241410525, 35.00000000000000000 ) ) ;
#839 = DIRECTION ( 'NONE',  ( 0.3420201433256481738, -0.9396926207859158664, 0.000000000000000000 ) ) ;
#840 = DIRECTION ( 'NONE',  ( 0.000000000000000000, 0.000000000000000000, 1.000000000000000000 ) ) ;
#841 = AXIS2_PLACEMENT_3D ( 'NONE', #6547, #3474, #17867 ) ;
#842 = EDGE_LOOP ( 'NONE', ( #4394, #7797, #7453, #15371 ) ) ;
#843 = CARTESIAN_POINT ( 'NONE',  ( -123.4618227840623632, -151.5628872026273086, -18.23991632971910093 ) ) ;
#844 = DIRECTION ( 'NONE',  ( 0.000000000000000000, 0.000000000000000000, -1.000000000000000000 ) ) ;
#845 = VERTEX_POINT ( 'NONE', #8981 ) ;
#846 = DIRECTION ( 'NONE',  ( -0.9396926207859069846, 0.3420201433256723766, 1.086737899652988166E-16 ) ) ;
#847 = FACE_OUTER_BOUND ( 'NONE', #13419, .T. ) ;
#848 = VERTEX_POINT ( 'NONE', #11435 ) ;
#849 = AXIS2_PLACEMENT_3D ( 'NONE', #13326, #7699, #1906 ) ;
#850 = VERTEX_POINT ( 'NONE', #6064 ) ;
#851 = UNCERTAINTY_MEASURE_WITH_UNIT (LENGTH_MEASURE( 1.000000000000000082E-05 ), #7064, 'distance_accuracy_value', 'NONE');
#852 = DIRECTION ( 'NONE',  ( 0.000000000000000000, 0.000000000000000000, 1.000000000000000000 ) ) ;
#853 = DIRECTION ( 'NONE',  ( 0.000000000000000000, 1.000000000000000000, -0.000000000000000000 ) ) ;
#854 = LINE ( 'NONE', #17968, #13566 ) ;
#855 = DIRECTION ( 'NONE',  ( 1.000000000000000000, 0.000000000000000000, 5.551115123125786646E-16 ) ) ;
#856 = CARTESIAN_POINT ( 'NONE',  ( -68.12361985383350316, 84.22855780814606419, 68.73600986863397111 ) ) ;
#857 = VERTEX_POINT ( 'NONE', #3093 ) ;
#858 = VECTOR ( 'NONE', #7679, 999.9999999999998863 ) ;
#859 = CARTESIAN_POINT ( 'NONE',  ( -50.78804881079258848, 75.44273092821050852, 15.00000000000006928 ) ) ;
#860 = DIRECTION ( 'NONE',  ( 0.000000000000000000, 0.000000000000000000, 1.000000000000000000 ) ) ;
#862 = ORIENTED_EDGE ( 'NONE', *, *, #18382, .T. ) ;
#861 = CARTESIAN_POINT ( 'NONE',  ( -78.11930149659737310, 84.72093613475881568, 55.01209040269093720 ) ) ;
#863 = CARTESIAN_POINT ( 'NONE',  ( -68.99615306438110451, 5.151604338130280070, 15.00000000000006928 ) ) ;
#864 = VERTEX_POINT ( 'NONE', #11793 ) ;
#865 = CARTESIAN_POINT ( 'NONE',  ( -71.24615306438070661, 141.0590213152292449, -167.1454815528550739 ) ) ;
#866 = ORIENTED_EDGE ( 'NONE', *, *, #15274, .T. ) ;
#867 = B_SPLINE_CURVE_WITH_KNOTS ( 'NONE', 3,
 ( #14957, #763, #6351, #1047, #10957, #8142, #9362, #2435, #16641, #15059, #7957, #5140, #10857, #13758, #16454, #9455, #18156, #6644, #12083, #12462 ),
 .UNSPECIFIED., .F., .F.,
 ( 4, 2, 2, 2, 2, 2, 2, 2, 2, 4 ),
 ( -1.439925654488394098E-05, 0.0006244272253376518481, 0.001263253707220187783, 0.002540906670985255533, 0.003818559634750323065, 0.005096212598515390164, 0.006373865562280457697, 0.007651518526045524363, 0.008929171489810592763, 0.01020682445357565943 ),
 .UNSPECIFIED. ) ;
#868 = FACE_OUTER_BOUND ( 'NONE', #12414, .T. ) ;
#869 = ORIENTED_EDGE ( 'NONE', *, *, #6051, .T. ) ;
#870 = AXIS2_PLACEMENT_3D ( 'NONE', #11609, #12763, #7219 ) ;
#871 = EDGE_CURVE ( 'NONE', #11023, #3553, #4318, .T. ) ;
#872 = EDGE_LOOP ( 'NONE', ( #7610, #14353 ) ) ;
#873 = DIRECTION ( 'NONE',  ( 1.000000000000000000, 2.062304371594500494E-16, 0.000000000000000000 ) ) ;
#874 = CARTESIAN_POINT ( 'NONE',  ( -38.92363814577095837, 71.26406042838981136, 97.49999999999998579 ) ) ;
#875 = CARTESIAN_POINT ( 'NONE',  ( -70.71978124295696944, -96.08423613455721579, 5.204170427930421283E-15 ) ) ;
#876 = ORIENTED_EDGE ( 'NONE', *, *, #587, .F. ) ;
#877 = DIRECTION ( 'NONE',  ( 1.000000000000000000, 2.062304371594500494E-16, -2.775557561562890858E-16 ) ) ;
#878 = ORIENTED_EDGE ( 'NONE', *, *, #12466, .F. ) ;
#879 = DIRECTION ( 'NONE',  ( -1.000000000000000000, 0.000000000000000000, 0.000000000000000000 ) ) ;
#880 = CARTESIAN_POINT ( 'NONE',  ( -123.4618227840623632, -111.0842361345572158, 57.00000000000000000 ) ) ;
#881 = VERTEX_POINT ( 'NONE', #4402 ) ;
#882 = AXIS2_PLACEMENT_3D ( 'NONE', #13146, #12986, #164 ) ;
#883 = CARTESIAN_POINT ( 'NONE',  ( -72.81448312412459245, 109.0309132574646469, -22.65846447477133196 ) ) ;
#884 = CARTESIAN_POINT ( 'NONE',  ( 4.699999999999995737, 0.000000000000000000, 0.000000000000000000 ) ) ;
#885 = VERTEX_POINT ( 'NONE', #5803 ) ;
#886 = VECTOR ( 'NONE', #5156, 999.9999999999998863 ) ;
#887 = DIRECTION ( 'NONE',  ( 0.000000000000000000, 0.000000000000000000, -1.000000000000000000 ) ) ;
#888 = CARTESIAN_POINT ( 'NONE',  ( -81.11364370225096820, -91.08930958056581062, -39.31393734470488255 ) ) ;
#889 = VERTEX_POINT ( 'NONE', #11533 ) ;
#890 = EDGE_CURVE ( 'NONE', #6749, #1925, #15737, .T. ) ;
#891 = ORIENTED_EDGE ( 'NONE', *, *, #12147, .T. ) ;
#892 = AXIS2_PLACEMENT_3D ( 'NONE', #1155, #10880, #1247 ) ;
#893 = CARTESIAN_POINT ( 'NONE',  ( 4.699999999999995737, 3.752776749732559924, -6.500000000000061284 ) ) ;
#894 = LINE ( 'NONE', #16235, #100 ) ;
#895 = ORIENTED_EDGE ( 'NONE', *, *, #333, .F. ) ;
#896 = DIRECTION ( 'NONE',  ( -1.000000000000000000, 0.000000000000000000, 0.000000000000000000 ) ) ;
#897 = CARTESIAN_POINT ( 'NONE',  ( -77.01756027604902499, 77.49305091727374872, 65.83480828159299847 ) ) ;
#898 = VECTOR ( 'NONE', #16815, 1000.000000000000000 ) ;
#899 = CARTESIAN_POINT ( 'NONE',  ( -92.59262256747318531, 0.3328663868096687350, 25.00000000000000000 ) ) ;
#900 = DIRECTION ( 'NONE',  ( 1.000000000000000000, 0.000000000000000000, 0.000000000000000000 ) ) ;
#901 = ORIENTED_EDGE ( 'NONE', *, *, #13495, .T. ) ;
#902 = B_SPLINE_CURVE_WITH_KNOTS ( 'NONE', 3,
 ( #11513, #2811, #7287, #2981 ),
 .UNSPECIFIED., .F., .F.,
 ( 4, 4 ),
 ( 0.000000000000000000, 0.002699315152504066541 ),
 .UNSPECIFIED. ) ;
#903 = EDGE_CURVE ( 'NONE', #18067, #18272, #17218, .T. ) ;
#904 = FACE_BOUND ( 'NONE', #13164, .T. ) ;
#905 = FACE_OUTER_BOUND ( 'NONE', #13588, .T. ) ;
#906 = CARTESIAN_POINT ( 'NONE',  ( -67.59262256747319952, 110.5691553257988460, 30.35917033480640370 ) ) ;
#907 = EDGE_CURVE ( 'NONE', #9806, #11339, #8716, .T. ) ;
#908 = CARTESIAN_POINT ( 'NONE',  ( 9.543663295069050534, 56.41207303426870112, 7.000000000000010658 ) ) ;
#909 = CARTESIAN_POINT ( 'NONE',  ( -107.5926225674731853, 114.3311569208253786, -25.00000000000000000 ) ) ;
#910 = ORIENTED_EDGE ( 'NONE', *, *, #13180, .T. ) ;
#911 = VECTOR ( 'NONE', #6055, 1000.000000000000000 ) ;
#912 = DIRECTION ( 'NONE',  ( 1.000000000000000000, 0.000000000000000000, -1.434969136109119680E-16 ) ) ;
#913 = FACE_OUTER_BOUND ( 'NONE', #3223, .T. ) ;
#914 = AXIS2_PLACEMENT_3D ( 'NONE', #4475, #8427, #7036 ) ;
#915 = ORIENTED_EDGE ( 'NONE', *, *, #2895, .F. ) ;
#916 = DIRECTION ( 'NONE',  ( -1.000000000000000000, 0.000000000000000000, -0.000000000000000000 ) ) ;
#918 = ADVANCED_FACE ( 'NONE', ( #16269 ), #6147, .T. ) ;
#917 = VECTOR ( 'NONE', #6803, 1000.000000000000000 ) ;
#919 =( NAMED_UNIT ( * ) PLANE_ANGLE_UNIT ( ) SI_UNIT ( $, .RADIAN. ) );
#920 = ORIENTED_EDGE ( 'NONE', *, *, #3325, .F. ) ;
#921 = VECTOR ( 'NONE', #6892, 1000.000000000000000 ) ;
#922 = EDGE_CURVE ( 'NONE', #10354, #6955, #14771, .T. ) ;
#923 = ORIENTED_EDGE ( 'NONE', *, *, #11202, .T. ) ;
#924 = EDGE_CURVE ( 'NONE', #6138, #3111, #9170, .T. ) ;
#925 = CARTESIAN_POINT ( 'NONE',  ( -57.08002265617300708, 84.22855780814606419, -167.1454815528550739 ) ) ;
#926 = ORIENTED_EDGE ( 'NONE', *, *, #14093, .F. ) ;
#927 = CARTESIAN_POINT ( 'NONE',  ( -66.75350761719796822, 56.49772428296282811, 24.14382665953563745 ) ) ;
#928 = LINE ( 'NONE', #6630, #98 ) ;
#929 = CARTESIAN_POINT ( 'NONE',  ( -66.56081925660646448, 59.51305259755623212, -27.99999999999999645 ) ) ;
#930 = EDGE_CURVE ( 'NONE', #5159, #18464, #2044, .T. ) ;
#931 = EDGE_CURVE ( 'NONE', #505, #8038, #6442, .T. ) ;
#932 = CARTESIAN_POINT ( 'NONE',  ( -171.0109138863553824, 84.22855780814606419, 55.00000000000000711 ) ) ;
#933 = VECTOR ( 'NONE', #4425, 1000.000000000000000 ) ;
#934 = EDGE_CURVE ( 'NONE', #15744, #1208, #5522, .T. ) ;
#935 = VECTOR ( 'NONE', #17439, 1000.000000000000114 ) ;
#936 = CARTESIAN_POINT ( 'NONE',  ( -68.99615306438094819, 64.22700883166265839, -167.1454815528550739 ) ) ;
#937 = DIRECTION ( 'NONE',  ( -1.000000000000000000, 1.760281407957729384E-14, 1.692578276882432005E-16 ) ) ;
#938 = ORIENTED_EDGE ( 'NONE', *, *, #890, .F. ) ;
#939 = EDGE_CURVE ( 'NONE', #10198, #60, #13560, .T. ) ;
#940 = DIRECTION ( 'NONE',  ( 1.000000000000000000, 0.000000000000000000, 0.000000000000000000 ) ) ;
#941 = B_SPLINE_CURVE_WITH_KNOTS ( 'NONE', 3,
 ( #7293, #1757, #10102, #8611, #7381, #17372 ),
 .UNSPECIFIED., .F., .F.,
 ( 4, 2, 4 ),
 ( 0.01067228061038553305, 0.01257272967564230723, 0.01447317874089908314 ),
 .UNSPECIFIED. ) ;
#942 = DIRECTION ( 'NONE',  ( 1.000000000000000000, -0.000000000000000000, -0.000000000000000000 ) ) ;
#943 = ORIENTED_EDGE ( 'NONE', *, *, #13071, .T. ) ;
#944 = AXIS2_PLACEMENT_3D ( 'NONE', #10386, #13473, #15913 ) ;
#945 = DIRECTION ( 'NONE',  ( 0.3420201433256407353, -0.9396926207859186420, 0.000000000000000000 ) ) ;
#946 = DIRECTION ( 'NONE',  ( -0.000000000000000000, 0.000000000000000000, 1.000000000000000000 ) ) ;
#947 = ORIENTED_EDGE ( 'NONE', *, *, #13616, .T. ) ;
#948 = EDGE_LOOP ( 'NONE', ( #10716, #16047, #16495, #5680 ) ) ;
#949 = VECTOR ( 'NONE', #12099, 1000.000000000000000 ) ;
#950 = VECTOR ( 'NONE', #1065, 1000.000000000000000 ) ;
#951 = ADVANCED_FACE ( 'NONE', ( #5030 ), #13463, .F. ) ;
#952 = EDGE_CURVE ( 'NONE', #12358, #17935, #14770, .T. ) ;
#953 = ORIENTED_EDGE ( 'NONE', *, *, #16934, .T. ) ;
#954 = CYLINDRICAL_SURFACE ( 'NONE', #402, 12.49999999999999112 ) ;
#955 = CARTESIAN_POINT ( 'NONE',  ( -57.08002265617300708, 84.22855780814606419, -15.00000000000001421 ) ) ;
#956 = CARTESIAN_POINT ( 'NONE',  ( -71.24615306438097662, 57.12489050456376560, -15.00000000000001421 ) ) ;
#957 = DIRECTION ( 'NONE',  ( -0.9396926207859084279, 0.3420201433256686574, 0.000000000000000000 ) ) ;
#958 = CIRCLE ( 'NONE', #8121, 4.599999999999992539 ) ;
#959 = CARTESIAN_POINT ( 'NONE',  ( -46.95762973216378811, 85.83453492254348305, -167.1454815528550739 ) ) ;
#960 = DIRECTION ( 'NONE',  ( 0.000000000000000000, 0.000000000000000000, -1.000000000000000000 ) ) ;
#961 = VERTEX_POINT ( 'NONE', #2238 ) ;
#962 = CARTESIAN_POINT ( 'NONE',  ( -57.89103256796045116, 73.45256821284057480, -15.00000000000001421 ) ) ;
#963 = CARTESIAN_POINT ( 'NONE',  ( -123.4618227840623632, -151.5628872026273086, 57.00000000000000000 ) ) ;
#965 = ORIENTED_EDGE ( 'NONE', *, *, #11845, .T. ) ;
#964 = CARTESIAN_POINT ( 'NONE',  ( -77.95646096175848072, 86.88560906486408442, 69.51788182020753482 ) ) ;
#966 = CARTESIAN_POINT ( 'NONE',  ( -115.7702289486888247, -96.08423613455721579, 5.654315315325360913 ) ) ;
#967 = AXIS2_PLACEMENT_3D ( 'NONE', #11022, #11220, #4101 ) ;
#968 = AXIS2_PLACEMENT_3D ( 'NONE', #2909, #3074, #1413 ) ;
#969 = LINE ( 'NONE', #17982, #8971 ) ;
#970 = ORIENTED_EDGE ( 'NONE', *, *, #15172, .F. ) ;
#971 = ORIENTED_EDGE ( 'NONE', *, *, #11111, .T. ) ;
#972 = EDGE_CURVE ( 'NONE', #13894, #9284, #1056, .T. ) ;
#973 = ORIENTED_EDGE ( 'NONE', *, *, #8614, .T. ) ;
#974 = AXIS2_PLACEMENT_3D ( 'NONE', #4166, #8475, #15486 ) ;
#975 = AXIS2_PLACEMENT_3D ( 'NONE', #12188, #9288, #4882 ) ;
#976 = CYLINDRICAL_SURFACE ( 'NONE', #17426, 45.40389983439752086 ) ;
#977 = FACE_OUTER_BOUND ( 'NONE', #9258, .T. ) ;
#978 = ORIENTED_EDGE ( 'NONE', *, *, #7449, .T. ) ;
#979 = DIRECTION ( 'NONE',  ( 1.000000000000000000, 0.000000000000000000, 0.000000000000000000 ) ) ;
#980 = CARTESIAN_POINT ( 'NONE',  ( -97.59262256747319952, 110.5691553257988460, 26.35917033480641436 ) ) ;
#981 = ORIENTED_EDGE ( 'NONE', *, *, #2192, .T. ) ;
#982 = VECTOR ( 'NONE', #13264, 1000.000000000000000 ) ;
#983 = LINE ( 'NONE', #5281, #7196 ) ;
#984 = CARTESIAN_POINT ( 'NONE',  ( -68.99615306438100504, 42.85071613813029501, -15.00000000000001421 ) ) ;
#985 = CARTESIAN_POINT ( 'NONE',  ( -53.84898691462515785, 93.95493478196527803, -167.1454815528550739 ) ) ;
#986 = ORIENTED_EDGE ( 'NONE', *, *, #12489, .F. ) ;
#987 = CARTESIAN_POINT ( 'NONE',  ( -74.24593559006332555, 108.0616442416786640, -23.22608149512904063 ) ) ;
#988 = CARTESIAN_POINT ( 'NONE',  ( -71.24615306438091977, 75.97444640456376419, 15.00000000000006928 ) ) ;
#990 = ORIENTED_EDGE ( 'NONE', *, *, #15850, .T. ) ;
#989 = EDGE_CURVE ( 'NONE', #1289, #768, #13897, .T. ) ;
#991 = VECTOR ( 'NONE', #5970, 1000.000000000000000 ) ;
#992 = DIRECTION ( 'NONE',  ( 0.000000000000000000, 0.000000000000000000, 1.000000000000000000 ) ) ;
#993 = EDGE_CURVE ( 'NONE', #9785, #3688, #10294, .T. ) ;
#994 = DIRECTION ( 'NONE',  ( -0.000000000000000000, -1.000000000000000000, -0.000000000000000000 ) ) ;
#995 = ORIENTED_EDGE ( 'NONE', *, *, #7003, .T. ) ;
#996 = VERTEX_POINT ( 'NONE', #13656 ) ;
#997 = AXIS2_PLACEMENT_3D ( 'NONE', #1387, #2599, #12718 ) ;
#998 = ORIENTED_EDGE ( 'NONE', *, *, #15679, .F. ) ;
#999 = CARTESIAN_POINT ( 'NONE',  ( -54.95363092160842911, 73.63336328296981037, -15.00000000000001421 ) ) ;
#1000 = VERTEX_POINT ( 'NONE', #5126 ) ;
#1001 = AXIS2_PLACEMENT_3D ( 'NONE', #7374, #17460, #2978 ) ;
#1002 = AXIS2_PLACEMENT_3D ( 'NONE', #14462, #1461, #10148 ) ;
#1003 = DIRECTION ( 'NONE',  ( 0.000000000000000000, 0.000000000000000000, 1.000000000000000000 ) ) ;
#1005 = VECTOR ( 'NONE', #11411, 1000.000000000000114 ) ;
#1004 = CARTESIAN_POINT ( 'NONE',  ( -77.85981289659012816, 80.89962780276930232, 55.77475785633962602 ) ) ;
#1006 = FACE_OUTER_BOUND ( 'NONE', #11409, .T. ) ;
#1007 = CARTESIAN_POINT ( 'NONE',  ( -123.4618227840623632, -111.0842361345572158, 57.00000000000000000 ) ) ;
#1008 = ORIENTED_EDGE ( 'NONE', *, *, #10694, .T. ) ;
#1009 = CARTESIAN_POINT ( 'NONE',  ( -92.59262256747321373, 117.8748711238780515, 25.00000000000000000 ) ) ;
#1010 = CARTESIAN_POINT ( 'NONE',  ( -112.5926225674731995, 50.58224449241410525, 35.00000000000000000 ) ) ;
#1011 = DIRECTION ( 'NONE',  ( 0.000000000000000000, 1.000000000000000000, 0.000000000000000000 ) ) ;
#1012 = CARTESIAN_POINT ( 'NONE',  ( -107.5926225674732137, 107.8748711238780373, 35.00000000000000000 ) ) ;
#1013 = ORIENTED_EDGE ( 'NONE', *, *, #11348, .F. ) ;
#1014 = AXIS2_PLACEMENT_3D ( 'NONE', #667, #4964, #5050 ) ;
#1015 = CARTESIAN_POINT ( 'NONE',  ( -60.06546592763143622, -91.08423613455721579, 38.97384619189705290 ) ) ;
#1016 = CARTESIAN_POINT ( 'NONE',  ( -63.40980125876075135, -92.35432432510552303, 43.13417342538335930 ) ) ;
#1017 = EDGE_LOOP ( 'NONE', ( #4962, #4427, #3232, #11663 ) ) ;
#1018 = AXIS2_PLACEMENT_3D ( 'NONE', #18076, #8156, #2447 ) ;
#1019 = LINE ( 'NONE', #2037, #18246 ) ;
#1020 = CIRCLE ( 'NONE', #6697, 9.999999999999994671 ) ;
#1021 = FACE_OUTER_BOUND ( 'NONE', #2125, .T. ) ;
#1022 = VERTEX_POINT ( 'NONE', #17767 ) ;
#1023 = VECTOR ( 'NONE', #12613, 1000.000000000000000 ) ;
#1024 = VERTEX_POINT ( 'NONE', #834 ) ;
#1025 = EDGE_CURVE ( 'NONE', #16752, #1935, #2548, .T. ) ;
#1026 = CARTESIAN_POINT ( 'NONE',  ( 103.5381772159376084, -151.5628872026272802, 57.00000000000000000 ) ) ;
#1027 = AXIS2_PLACEMENT_3D ( 'NONE', #13141, #17251, #1911 ) ;
#1028 = ORIENTED_EDGE ( 'NONE', *, *, #8577, .F. ) ;
#1029 = CARTESIAN_POINT ( 'NONE',  ( -67.37336793441032512, 56.72162401922281560, 22.91103267187422787 ) ) ;
#1030 = DIRECTION ( 'NONE',  ( -0.9396926207859022107, 0.3420201433256853663, 0.000000000000000000 ) ) ;
#1031 = CARTESIAN_POINT ( 'NONE',  ( -68.99615306438069240, 121.3905323881302678, 15.00000000000006928 ) ) ;
#1032 = VECTOR ( 'NONE', #279, 1000.000000000000000 ) ;
#1033 = DIRECTION ( 'NONE',  ( -0.9915318908039647550, 1.590368294782254281E-17, -0.1298634264091108326 ) ) ;
#1034 = AXIS2_PLACEMENT_3D ( 'NONE', #3289, #4973, #4881 ) ;
#1035 = CIRCLE ( 'NONE', #6718, 10.24900000000000055 ) ;
#1036 = CARTESIAN_POINT ( 'NONE',  ( 0.1061556211655283882, 6.421950209808267473, 1.876855952934465721 ) ) ;
#1037 = DIRECTION ( 'NONE',  ( 0.000000000000000000, -5.551115123125748189E-17, -1.000000000000000000 ) ) ;
#1038 = CARTESIAN_POINT ( 'NONE',  ( -0.000000000000000000, -111.0842361345572158, -3.000000000000000000 ) ) ;
#1039 = PRODUCT_DEFINITION_SHAPE ( 'NONE', 'NONE',  #18527 ) ;
#1040 = ORIENTED_EDGE ( 'NONE', *, *, #11176, .F. ) ;
#1041 = EDGE_CURVE ( 'NONE', #13411, #11585, #10588, .T. ) ;
#1042 = EDGE_CURVE ( 'NONE', #9640, #3596, #2530, .T. ) ;
#1043 = DIRECTION ( 'NONE',  ( 0.000000000000000000, 1.000000000000000000, -0.000000000000000000 ) ) ;
#1044 = DIRECTION ( 'NONE',  ( -1.000000000000000000, 0.000000000000000000, -0.000000000000000000 ) ) ;
#1045 = VERTEX_POINT ( 'NONE', #13291 ) ;
#1046=STYLED_ITEM('',(#18559),#257);
#1047 = CARTESIAN_POINT ( 'NONE',  ( -31.06841040534018106, -91.10977296152353233, -10.13292952605206310 ) ) ;
#1048 = CARTESIAN_POINT ( 'NONE',  ( -71.24615306438080609, 104.2487802545637408, -15.00000000000001421 ) ) ;
#1049 = ORIENTED_EDGE ( 'NONE', *, *, #15194, .T. ) ;
#1050 = EDGE_LOOP ( 'NONE', ( #14252, #1714, #1805 ) ) ;
#1051 = AXIS2_PLACEMENT_3D ( 'NONE', #2696, #6904, #5499 ) ;
#1052 = EDGE_CURVE ( 'NONE', #6388, #2078, #4951, .T. ) ;
#1053 = EDGE_CURVE ( 'NONE', #17316, #9785, #16350, .T. ) ;
#1054 = AXIS2_PLACEMENT_3D ( 'NONE', #5183, #18105, #10990 ) ;
#1055 = ADVANCED_FACE ( 'NONE', ( #3537 ), #14940, .T. ) ;
#1056 = CIRCLE ( 'NONE', #11519, 10.24900000000000055 ) ;
#1057 = ORIENTED_EDGE ( 'NONE', *, *, #13713, .F. ) ;
#1058 = UNCERTAINTY_MEASURE_WITH_UNIT (LENGTH_MEASURE( 1.000000000000000082E-05 ), #12203, 'distance_accuracy_value', 'NONE');
#1059 = CARTESIAN_POINT ( 'NONE',  ( -64.09025127992789805, 117.8748711238780089, 7.000000000000010658 ) ) ;
#1060 = CARTESIAN_POINT ( 'NONE',  ( -57.08002265617300708, 84.22855780814606419, -15.00000000000001421 ) ) ;
#1061 = PLANE ( 'NONE',  #11505 ) ;
#1062 = CARTESIAN_POINT ( 'NONE',  ( -107.5926225674731711, 57.88796029049330372, 26.35917033480641436 ) ) ;
#1063 = EDGE_CURVE ( 'NONE', #3060, #4, #4507, .T. ) ;
#1064 = CARTESIAN_POINT ( 'NONE',  ( -68.99615306438100504, 45.37745293166267402, -15.00000000000001421 ) ) ;
#1065 = DIRECTION ( 'NONE',  ( -0.9396926207859167546, 0.3420201433256456203, 1.086737899652999506E-16 ) ) ;
#1066 = ORIENTED_EDGE ( 'NONE', *, *, #5722, .T. ) ;
#1067 = VECTOR ( 'NONE', #16551, 1000.000000000000000 ) ;
#1068 = DIRECTION ( 'NONE',  ( 1.000000000000000000, 0.000000000000000000, 0.000000000000000000 ) ) ;
#1069 = CARTESIAN_POINT ( 'NONE',  ( -112.5926225674731853, 50.58224449241410525, 15.00000000000004796 ) ) ;
#1071 = EDGE_LOOP ( 'NONE', ( #14079, #1438 ) ) ;
#1070 = CARTESIAN_POINT ( 'NONE',  ( -77.35494310313409017, 89.87539756129700663, 67.45979609325928550 ) ) ;
#1072 = DIRECTION ( 'NONE',  ( 0.000000000000000000, 0.000000000000000000, 1.000000000000000000 ) ) ;
#1073 = AXIS2_PLACEMENT_3D ( 'NONE', #12166, #16356, #2049 ) ;
#1074 = EDGE_CURVE ( 'NONE', #7990, #15187, #15432, .T. ) ;
#1075 = VECTOR ( 'NONE', #6731, 1000.000000000000114 ) ;
#1076 = EDGE_CURVE ( 'NONE', #6989, #4422, #2617, .T. ) ;
#1077 = DIRECTION ( 'NONE',  ( 0.9396926207859135349, 0.3420201433256546686, 0.000000000000000000 ) ) ;
#1078 = ORIENTED_EDGE ( 'NONE', *, *, #12131, .F. ) ;
#1079 = DIRECTION ( 'NONE',  ( 0.000000000000000000, 0.000000000000000000, -1.000000000000000000 ) ) ;
#1080 = EDGE_LOOP ( 'NONE', ( #7717, #7540 ) ) ;
#1081 = EDGE_CURVE ( 'NONE', #3688, #13603, #10947, .T. ) ;
#1082 = ORIENTED_EDGE ( 'NONE', *, *, #6863, .T. ) ;
#1083 = VECTOR ( 'NONE', #15801, 1000.000000000000000 ) ;
#1084 = VECTOR ( 'NONE', #5911, 1000.000000000000000 ) ;
#1085 = DIRECTION ( 'NONE',  ( -1.000000000000000000, 6.033820786006277040E-15, 0.000000000000000000 ) ) ;
#1086 = CARTESIAN_POINT ( 'NONE',  ( 9.543663295069050534, 56.41207303426870112, -7.000000000000010658 ) ) ;
#1087 = CARTESIAN_POINT ( 'NONE',  ( -70.71978124295668522, -96.08423613455721579, -17.52877280353970235 ) ) ;
#1088 = EDGE_LOOP ( 'NONE', ( #7238, #671, #17616, #2992 ) ) ;
#1089 = CARTESIAN_POINT ( 'NONE',  ( -30.06971094502080177, -91.24992749556385263, 9.348345296714491326 ) ) ;
#1090 = DIRECTION ( 'NONE',  ( 0.000000000000000000, 0.000000000000000000, 1.000000000000000000 ) ) ;
#1091 = ORIENTED_EDGE ( 'NONE', *, *, #16945, .T. ) ;
#1092 = CARTESIAN_POINT ( 'NONE',  ( -100.4870060002411805, -151.5628872026273086, 18.23991632971911514 ) ) ;
#1093 = FACE_OUTER_BOUND ( 'NONE', #6815, .T. ) ;
#1094 = LINE ( 'NONE', #12504, #13236 ) ;
#1095 = ORIENTED_EDGE ( 'NONE', *, *, #8907, .T. ) ;
#1096 = CARTESIAN_POINT ( 'NONE',  ( -75.82627924895463423, 106.8366279053472283, -27.81200583293166417 ) ) ;
#1097 = CYLINDRICAL_SURFACE ( 'NONE', #4269, 7.168074330098680669 ) ;
#1098 = CARTESIAN_POINT ( 'NONE',  ( -71.24615306438103346, 40.52805651522925245, -15.00000000000001421 ) ) ;
#1099 = DIRECTION ( 'NONE',  ( 0.000000000000000000, 1.000000000000000000, 0.000000000000000000 ) ) ;
#1100 = ORIENTED_EDGE ( 'NONE', *, *, #2868, .T. ) ;
#1101 = VERTEX_POINT ( 'NONE', #4112 ) ;
#1102 = DIRECTION ( 'NONE',  ( 1.000000000000000000, 0.000000000000000000, 5.077734830647306615E-16 ) ) ;
#1103 = CARTESIAN_POINT ( 'NONE',  ( 0.000000000000000000, 0.000000000000000000, 0.000000000000000000 ) ) ;
#1104 = ORIENTED_EDGE ( 'NONE', *, *, #9720, .F. ) ;
#1105 = DIRECTION ( 'NONE',  ( -0.9475106458593564041, 0.3197242186372270534, -0.000000000000000000 ) ) ;
#1106 = CARTESIAN_POINT ( 'NONE',  ( -71.24615306438109030, 24.82009326522924297, 15.00000000000006928 ) ) ;
#1107 = DIRECTION ( 'NONE',  ( 0.3420201433256481738, -0.9396926207859158664, 0.000000000000000000 ) ) ;
#1108 = DIRECTION ( 'NONE',  ( 0.000000000000000000, 0.000000000000000000, 1.000000000000000000 ) ) ;
#1109 = ORIENTED_EDGE ( 'NONE', *, *, #1727, .T. ) ;
#1110 = LINE ( 'NONE', #13923, #617 ) ;
#1111 = FACE_OUTER_BOUND ( 'NONE', #17441, .T. ) ;
#1112 = CARTESIAN_POINT ( 'NONE',  ( -68.99615306438117557, 1.395155831662692192, -15.00000000000001421 ) ) ;
#1113 = CARTESIAN_POINT ( 'NONE',  ( 5.233202738124664855, -19.34983604512936495, -54.79921157549230770 ) ) ;
#1114 = CARTESIAN_POINT ( 'NONE',  ( -6.009442422294567265, 35.67642109510119752, 36.02332778080708664 ) ) ;
#1115 = VERTEX_POINT ( 'NONE', #16826 ) ;
#1116 = CARTESIAN_POINT ( 'NONE',  ( -62.67046908522836191, -91.80659809767264790, 42.25010775664332385 ) ) ;
#1117 = FACE_OUTER_BOUND ( 'NONE', #1125, .T. ) ;
#1118 = CARTESIAN_POINT ( 'NONE',  ( -57.08002265617300708, 84.22855780814606419, -15.00000000000001421 ) ) ;
#1119 = VERTEX_POINT ( 'NONE', #15330 ) ;
#1120 = ORIENTED_EDGE ( 'NONE', *, *, #8674, .T. ) ;
#1121 = PLANE ( 'NONE',  #17134 ) ;
#1122 = LINE ( 'NONE', #8417, #18391 ) ;
#1123 = PLANE ( 'NONE',  #1879 ) ;
#1124 = LINE ( 'NONE', #7948, #12683 ) ;
#1125 = EDGE_LOOP ( 'NONE', ( #16868, #13231, #10617, #17298 ) ) ;
#1126 = CARTESIAN_POINT ( 'NONE',  ( 2.027458062547893923E-14, 0.6351314446023053062, -6.500000000000062172 ) ) ;
#1127 = CARTESIAN_POINT ( 'NONE',  ( -45.07766827056850190, 51.92519128693054142, 25.99195503995988688 ) ) ;
#1128 = DIRECTION ( 'NONE',  ( -0.000000000000000000, -1.000000000000000000, -0.000000000000000000 ) ) ;
#1129 = ORIENTED_EDGE ( 'NONE', *, *, #14826, .T. ) ;
#1130 = ADVANCED_FACE ( 'NONE', ( #18043 ), #13938, .T. ) ;
#1131 = DIRECTION ( 'NONE',  ( 1.156482317317869999E-16, 0.000000000000000000, 1.000000000000000000 ) ) ;
#1132 = CARTESIAN_POINT ( 'NONE',  ( -123.4618227840623632, -151.5628872026273086, 57.00000000000000000 ) ) ;
#1133 = EDGE_LOOP ( 'NONE', ( #5557, #3035, #10608, #2937 ) ) ;
#1134 = DIRECTION ( 'NONE',  ( 1.000000000000000000, 0.000000000000000000, 0.000000000000000000 ) ) ;
#1135 = DIRECTION ( 'NONE',  ( -1.000000000000000000, 0.000000000000000000, 0.000000000000000000 ) ) ;
#1136 = ORIENTED_EDGE ( 'NONE', *, *, #8714, .T. ) ;
#1137 = ORIENTED_EDGE ( 'NONE', *, *, #12714, .F. ) ;
#1138 = EDGE_CURVE ( 'NONE', #162, #13480, #1122, .T. ) ;
#1139 = ORIENTED_EDGE ( 'NONE', *, *, #4989, .F. ) ;
#1140 = EDGE_CURVE ( 'NONE', #9962, #16099, #6915, .T. ) ;
#1141 = DIRECTION ( 'NONE',  ( 0.000000000000000000, 0.000000000000000000, 1.000000000000000000 ) ) ;
#1142 = DIRECTION ( 'NONE',  ( -2.062304371594500494E-16, 1.000000000000000000, -0.000000000000000000 ) ) ;
#1143 = CARTESIAN_POINT ( 'NONE',  ( 45.30000000000000426, 0.000000000000000000, 0.000000000000000000 ) ) ;
#1144 = DIRECTION ( 'NONE',  ( 0.9396926207859110924, 0.3420201433256611634, 0.000000000000000000 ) ) ;
#1145 = CARTESIAN_POINT ( 'NONE',  ( -71.24615306438079188, 112.7846874652292399, -167.1454815528550739 ) ) ;
#1146 = CARTESIAN_POINT ( 'NONE',  ( -71.24615306438077766, 113.6735582045637045, -15.00000000000001421 ) ) ;
#1147 = ORIENTED_EDGE ( 'NONE', *, *, #13705, .T. ) ;
#1148 = EDGE_CURVE ( 'NONE', #15468, #8935, #14128, .T. ) ;
#1149 = DIRECTION ( 'NONE',  ( -1.000000000000000000, 0.000000000000000000, 0.000000000000000000 ) ) ;
#1150 = CARTESIAN_POINT ( 'NONE',  ( -94.45685920050698314, -47.21335801510345220, -15.00000000000001421 ) ) ;
#1152 = ORIENTED_EDGE ( 'NONE', *, *, #311, .T. ) ;
#1151 = PLANE ( 'NONE',  #16206 ) ;
#1153 = EDGE_CURVE ( 'NONE', #16485, #3472, #5228, .T. ) ;
#1154 = CARTESIAN_POINT ( 'NONE',  ( -71.24615306438070661, 187.7866419848965052, -167.1454815528550739 ) ) ;
#1155 = CARTESIAN_POINT ( 'NONE',  ( -102.4618227840623774, -111.0842361345572158, 36.00000000000000711 ) ) ;
#1156 = EDGE_LOOP ( 'NONE', ( #16086, #9240, #2898, #2982 ) ) ;
#1157 = CARTESIAN_POINT ( 'NONE',  ( -70.71978124295696944, -96.08423613455721579, 5.204170427930421283E-15 ) ) ;
#1158 = ORIENTED_EDGE ( 'NONE', *, *, #5375, .T. ) ;
#1159 = ADVANCED_FACE ( 'NONE', ( #3917 ), #13599, .T. ) ;
#1160 = EDGE_CURVE ( 'NONE', #14280, #401, #8316, .T. ) ;
#1161 = VERTEX_POINT ( 'NONE', #9914 ) ;
#1162 = EDGE_CURVE ( 'NONE', #5195, #5717, #8229, .T. ) ;
#1163 = EDGE_CURVE ( 'NONE', #13829, #10929, #1213, .T. ) ;
#1164 = AXIS2_PLACEMENT_3D ( 'NONE', #3751, #12553, #6745 ) ;
#1165 = LINE ( 'NONE', #7065, #14167 ) ;
#1166 = DIRECTION ( 'NONE',  ( 0.000000000000000000, 0.000000000000000000, 1.000000000000000000 ) ) ;
#1167 = VERTEX_POINT ( 'NONE', #12644 ) ;
#1168 = APPLICATION_PROTOCOL_DEFINITION ( 'draft international standard', 'automotive_design', 1998, #7518 ) ;
#1169 = ORIENTED_EDGE ( 'NONE', *, *, #11243, .T. ) ;
#1170 = CARTESIAN_POINT ( 'NONE',  ( -5.374518711846989483, 34.99587063685016375, -36.39809049692809850 ) ) ;
#1171 = LINE ( 'NONE', #5559, #1945 ) ;
#1172 = ORIENTED_EDGE ( 'NONE', *, *, #11434, .T. ) ;
#1173 = EDGE_CURVE ( 'NONE', #9439, #10991, #7622, .T. ) ;
#1174 = CARTESIAN_POINT ( 'NONE',  ( -71.24615306438079188, 113.6735582045637045, -15.00000000000001421 ) ) ;
#1175 = CARTESIAN_POINT ( 'NONE',  ( -67.59262256747319952, 111.6514400295689171, 22.50837044127971254 ) ) ;
#1176 = EDGE_CURVE ( 'NONE', #8598, #5018, #18146, .T. ) ;
#1177 = CARTESIAN_POINT ( 'NONE',  ( -68.99615306438074924, 121.3905323881302962, -15.00000000000001421 ) ) ;
#1178 = VERTEX_POINT ( 'NONE', #13742 ) ;
#1179 = CARTESIAN_POINT ( 'NONE',  ( -102.5926225674731853, 102.8748711238780373, -20.00000000000000355 ) ) ;
#1180 = DIRECTION ( 'NONE',  ( -1.000000000000000000, 0.000000000000000000, 0.000000000000000000 ) ) ;
#1181 = ORIENTED_EDGE ( 'NONE', *, *, #10655, .T. ) ;
#1182 = DIRECTION ( 'NONE',  ( 0.9396926207859097602, 0.3420201433256649937, -1.086737899652991371E-16 ) ) ;
#1183 = VECTOR ( 'NONE', #13108, 1000.000000000000114 ) ;
#1184 = CARTESIAN_POINT ( 'NONE',  ( -48.98198201484814263, 93.75072866207695199, -167.1454815528550739 ) ) ;
#1185 = ORIENTED_EDGE ( 'NONE', *, *, #12268, .T. ) ;
#1186 = ADVANCED_FACE ( 'NONE', ( #7022 ), #9528, .F. ) ;
#1187 = VERTEX_POINT ( 'NONE', #17461 ) ;
#1188 = EDGE_CURVE ( 'NONE', #18272, #5560, #346, .T. ) ;
#1189 = DIRECTION ( 'NONE',  ( 0.000000000000000000, 0.000000000000000000, -1.000000000000000000 ) ) ;
#1190 = EDGE_LOOP ( 'NONE', ( #11318, #6672, #1682, #10970 ) ) ;
#1191 = LINE ( 'NONE', #2388, #921 ) ;
#1192 = CARTESIAN_POINT ( 'NONE',  ( -53.44817431141344599, 74.64462966772957486, -167.1454815528550739 ) ) ;
#1193 = PLANE ( 'NONE',  #15871 ) ;
#1194 = VECTOR ( 'NONE', #8379, 1000.000000000000000 ) ;
#1195 = LINE ( 'NONE', #16991, #9386 ) ;
#1196 = ORIENTED_EDGE ( 'NONE', *, *, #12856, .T. ) ;
#1197 = LINE ( 'NONE', #5490, #8699 ) ;
#1198 = VECTOR ( 'NONE', #8394, 1000.000000000000000 ) ;
#1199 = DIRECTION ( 'NONE',  ( 1.000000000000000000, 0.000000000000000000, 0.000000000000000000 ) ) ;
#1200 = CARTESIAN_POINT ( 'NONE',  ( -75.73736374306625407, 106.9102428511424279, 24.71466311077380951 ) ) ;
#1201 = LINE ( 'NONE', #3900, #6019 ) ;
#1202 = LINE ( 'NONE', #15607, #11135 ) ;
#1203 = EDGE_LOOP ( 'NONE', ( #7524, #14271 ) ) ;
#1204 = CARTESIAN_POINT ( 'NONE',  ( -71.24615306438117557, 6.859408104563785358, -167.1454815528550739 ) ) ;
#1205 = DIRECTION ( 'NONE',  ( -2.062304371594500494E-16, 1.000000000000000000, 2.385018538676381657E-32 ) ) ;
#1206 = DIRECTION ( 'NONE',  ( -1.000000000000000000, 0.000000000000000000, 0.000000000000000000 ) ) ;
#1207 = CARTESIAN_POINT ( 'NONE',  ( -68.12361985383350316, 84.22855780814606419, 37.50000000000000000 ) ) ;
#1208 = VERTEX_POINT ( 'NONE', #5869 ) ;
#1209 = VECTOR ( 'NONE', #18271, 1000.000000000000000 ) ;
#1210 = ORIENTED_EDGE ( 'NONE', *, *, #3545, .T. ) ;
#1211 = CARTESIAN_POINT ( 'NONE',  ( 0.01372220897670155954, -5.948365447239731374, -2.697128823393899477 ) ) ;
#1212 = ORIENTED_EDGE ( 'NONE', *, *, #3868, .T. ) ;
#1213 = LINE ( 'NONE', #16630, #7917 ) ;
#1214 = DIRECTION ( 'NONE',  ( 0.000000000000000000, -0.000000000000000000, 1.000000000000000000 ) ) ;
#1215 = DIRECTION ( 'NONE',  ( 0.000000000000000000, 0.000000000000000000, 1.000000000000000000 ) ) ;
#1216 = ORIENTED_EDGE ( 'NONE', *, *, #17723, .T. ) ;
#1217 = CARTESIAN_POINT ( 'NONE',  ( 0.2595206531158619767, 2.531175536751702371, -6.500000000000062172 ) ) ;
#1218 = CARTESIAN_POINT ( 'NONE',  ( -57.08002265617300708, 84.22855780814606419, 25.00000000000000355 ) ) ;
#1219 = CARTESIAN_POINT ( 'NONE',  ( -71.24615306438094819, 66.54966845456371516, 15.00000000000006928 ) ) ;
#1220 = DIRECTION ( 'NONE',  ( 0.000000000000000000, 0.000000000000000000, 1.000000000000000000 ) ) ;
#1221 = EDGE_LOOP ( 'NONE', ( #3061, #6392, #5611, #17061 ) ) ;
#1222 = VECTOR ( 'NONE', #4657, 1000.000000000000000 ) ;
#1223 = CIRCLE ( 'NONE', #15253, 1.000000000000000888 ) ;
#1224 = AXIS2_PLACEMENT_3D ( 'NONE', #99, #12928, #17214 ) ;
#1225 = DIRECTION ( 'NONE',  ( 0.9396926207859171987, 0.3420201433256444545, -1.086737899652999999E-16 ) ) ;
#1226 = ORIENTED_EDGE ( 'NONE', *, *, #7620, .T. ) ;
#1227 = EDGE_CURVE ( 'NONE', #17762, #13685, #17235, .T. ) ;
#1228 = LINE ( 'NONE', #4398, #12878 ) ;
#1229 = DIRECTION ( 'NONE',  ( 1.156482317317869999E-16, 0.000000000000000000, 1.000000000000000000 ) ) ;
#1230 = VERTEX_POINT ( 'NONE', #14391 ) ;
#1231 = VERTEX_POINT ( 'NONE', #8604 ) ;
#1232 = VECTOR ( 'NONE', #3529, 1000.000000000000000 ) ;
#1233 = VECTOR ( 'NONE', #6721, 1000.000000000000114 ) ;
#1234 = ORIENTED_EDGE ( 'NONE', *, *, #5956, .F. ) ;
#1235 = UNCERTAINTY_MEASURE_WITH_UNIT (LENGTH_MEASURE( 1.000000000000000082E-05 ), #17113, 'distance_accuracy_value', 'NONE');
#1236 = CIRCLE ( 'NONE', #7215, 10.24900000000000055 ) ;
#1237 = CYLINDRICAL_SURFACE ( 'NONE', #13579, 5.654315315325682434 ) ;
#1238 = DIRECTION ( 'NONE',  ( 0.000000000000000000, 0.000000000000000000, 1.000000000000000000 ) ) ;
#1239 = DIRECTION ( 'NONE',  ( -1.000000000000000000, -0.000000000000000000, -0.000000000000000000 ) ) ;
#1240 = CARTESIAN_POINT ( 'NONE',  ( -31.03642545851250745, 84.22855780814606419, -47.49999999999999289 ) ) ;
#1241 = CARTESIAN_POINT ( 'NONE',  ( -83.23321842955245131, 73.26749283226919829, 92.50000000000000000 ) ) ;
#1242 = ORIENTED_EDGE ( 'NONE', *, *, #7340, .F. ) ;
#1243 = DIRECTION ( 'NONE',  ( 0.000000000000000000, 1.000000000000000000, 0.000000000000000000 ) ) ;
#1244 = ORIENTED_EDGE ( 'NONE', *, *, #8704, .T. ) ;
#1245 = CIRCLE ( 'NONE', #5995, 11.04359719766049430 ) ;
#1246 = DIRECTION ( 'NONE',  ( -0.9396926207859068736, 0.3420201433256726542, 1.086737899652988043E-16 ) ) ;
#1247 = DIRECTION ( 'NONE',  ( 6.608470384673552010E-16, 0.000000000000000000, -1.000000000000000000 ) ) ;
#1248 = EDGE_LOOP ( 'NONE', ( #2491, #7327, #310, #9857 ) ) ;
#1249 = ADVANCED_FACE ( 'NONE', ( #3068 ), #14305, .T. ) ;
#1250 = AXIS2_PLACEMENT_3D ( 'NONE', #6483, #12205, #17896 ) ;
#1251 = VECTOR ( 'NONE', #17613, 1000.000000000000000 ) ;
#1252 = CARTESIAN_POINT ( 'NONE',  ( -38.09490121289055509, 73.26749283227019305, 97.49999999999998579 ) ) ;
#1253 = VERTEX_POINT ( 'NONE', #10094 ) ;
#1254 = ORIENTED_EDGE ( 'NONE', *, *, #4048, .T. ) ;
#1255 = CIRCLE ( 'NONE', #12295, 95.91469608272775815 ) ;
#1256 = ADVANCED_FACE ( 'NONE', ( #15793 ), #17278, .T. ) ;
#1257 = CARTESIAN_POINT ( 'NONE',  ( -71.24615306438089135, 85.39922435456371375, -15.00000000000001421 ) ) ;
#1258 = DIRECTION ( 'NONE',  ( 0.000000000000000000, 8.876422075684827903E-15, -1.000000000000000000 ) ) ;
#1259 = ORIENTED_EDGE ( 'NONE', *, *, #8733, .F. ) ;
#1260 = CONTEXT_DEPENDENT_SHAPE_REPRESENTATION ( #10739, #7719 ) ;
#1261 = VERTEX_POINT ( 'NONE', #17913 ) ;
#1262 = AXIS2_PLACEMENT_3D ( 'NONE', #1972, #10573, #13375 ) ;
#1263 = CARTESIAN_POINT ( 'NONE',  ( -0.3548237229735157761, 28.74729804758344542, -39.59865668900319946 ) ) ;
#1264 = LINE ( 'NONE', #12691, #11810 ) ;
#1265 = ORIENTED_EDGE ( 'NONE', *, *, #2637, .F. ) ;
#1266 = DIRECTION ( 'NONE',  ( -1.000000000000000000, 0.000000000000000000, 0.000000000000000000 ) ) ;
#1267 = CARTESIAN_POINT ( 'NONE',  ( 276.3098885457529832, -32.62665103886256190, -3.000000000000000000 ) ) ;
#1268 = PLANE ( 'NONE',  #14700 ) ;
#1269 = EDGE_CURVE ( 'NONE', #13855, #11938, #442, .T. ) ;
#1270 = ORIENTED_EDGE ( 'NONE', *, *, #2418, .T. ) ;
#1271 = EDGE_CURVE ( 'NONE', #14048, #12123, #11852, .T. ) ;
#1272 = CARTESIAN_POINT ( 'NONE',  ( -75.66320186394305836, 106.9708331287094580, -24.59982859766222418 ) ) ;
#1273 = LINE ( 'NONE', #6877, #3065 ) ;
#1274 = ORIENTED_EDGE ( 'NONE', *, *, #4335, .T. ) ;
#1275 = EDGE_CURVE ( 'NONE', #6461, #5649, #7644, .T. ) ;
#1276 = CIRCLE ( 'NONE', #7821, 3.999999999999989786 ) ;
#1277 = CARTESIAN_POINT ( 'NONE',  ( -68.99615306438100504, 39.09426763166271002, -167.1454815528550739 ) ) ;
#1278 = DIRECTION ( 'NONE',  ( -0.9475106458593564041, -0.3197242186372270534, -0.000000000000000000 ) ) ;
#1279 = AXIS2_PLACEMENT_3D ( 'NONE', #14376, #3231, #11579 ) ;
#1280 = AXIS2_PLACEMENT_3D ( 'NONE', #10908, #15287, #15186 ) ;
#1281 = ORIENTED_EDGE ( 'NONE', *, *, #1838, .T. ) ;
#1282 = ORIENTED_EDGE ( 'NONE', *, *, #15902, .F. ) ;
#1283 = ADVANCED_FACE ( 'NONE', ( #14742 ), #14917, .T. ) ;
#1284 = ADVANCED_FACE ( 'NONE', ( #10445 ), #17638, .T. ) ;
#1285 = EDGE_CURVE ( 'NONE', #12345, #7975, #2857, .T. ) ;
#1286 = ORIENTED_EDGE ( 'NONE', *, *, #7547, .T. ) ;
#1287 = PLANE ( 'NONE',  #7582 ) ;
#1288 = CIRCLE ( 'NONE', #16496, 172.7605492041889192 ) ;
#1289 = VERTEX_POINT ( 'NONE', #7923 ) ;
#1290 = EDGE_CURVE ( 'NONE', #415, #13190, #3329, .T. ) ;
#1291 = CARTESIAN_POINT ( 'NONE',  ( -69.26024277767963611, 81.41924511788803898, -15.00000000000001243 ) ) ;
#1292 = DIRECTION ( 'NONE',  ( 0.000000000000000000, 0.000000000000000000, 1.000000000000000000 ) ) ;
#1293 = CARTESIAN_POINT ( 'NONE',  ( 113.3630170098442989, -111.0842361345572158, -7.000000000000010658 ) ) ;
#1294 = DIRECTION ( 'NONE',  ( -5.204170427930409450E-16, 0.000000000000000000, 1.000000000000000000 ) ) ;
#1295 = EDGE_LOOP ( 'NONE', ( #11443, #1864, #4182, #1863 ) ) ;
#1296 = ADVANCED_FACE ( 'NONE', ( #725 ), #811, .T. ) ;
#1297 = DIRECTION ( 'NONE',  ( 0.000000000000000000, 0.000000000000000000, 1.000000000000000000 ) ) ;
#1298 = VECTOR ( 'NONE', #12416, 1000.000000000000000 ) ;
#1299 = AXIS2_PLACEMENT_3D ( 'NONE', #11088, #17069, #11190 ) ;
#1300 = CARTESIAN_POINT ( 'NONE',  ( -50.06979403241810900, 50.58224449241409104, -26.91246033477409583 ) ) ;
#1301 = DIRECTION ( 'NONE',  ( -5.204170427930409450E-16, 0.000000000000000000, 1.000000000000000000 ) ) ;
#1302 = CARTESIAN_POINT ( 'NONE',  ( 14.89878123376213814, -10.86838903421133296, 53.26686714696702296 ) ) ;
#1303 = ORIENTED_EDGE ( 'NONE', *, *, #9270, .T. ) ;
#1304 = ADVANCED_FACE ( 'NONE', ( #2020 ), #13538, .T. ) ;
#1305 = FACE_OUTER_BOUND ( 'NONE', #5820, .T. ) ;
#1306 = CARTESIAN_POINT ( 'NONE',  ( -68.99615306438094819, 70.51019413166270056, -167.1454815528550739 ) ) ;
#1307 = EDGE_CURVE ( 'NONE', #800, #4074, #8827, .T. ) ;
#1308 = AXIS2_PLACEMENT_3D ( 'NONE', #1669, #8784, #9145 ) ;
#1309 = CARTESIAN_POINT ( 'NONE',  ( -68.99615306438077766, 123.9172691816626610, -167.1454815528550739 ) ) ;
#1310 = CARTESIAN_POINT ( 'NONE',  ( -71.24615306438086293, 87.65194626522927024, -15.00000000000001421 ) ) ;
#1311 = ORIENTED_EDGE ( 'NONE', *, *, #8334, .F. ) ;
#1312 = ORIENTED_EDGE ( 'NONE', *, *, #15097, .T. ) ;
#1313 = AXIS2_PLACEMENT_3D ( 'NONE', #12912, #7285, #17108 ) ;
#1314 = VECTOR ( 'NONE', #1694, 1000.000000000000000 ) ;
#1315 = AXIS2_PLACEMENT_3D ( 'NONE', #12349, #13837, #16264 ) ;
#1316 = CARTESIAN_POINT ( 'NONE',  ( -67.59262256747315689, 117.8748711238780373, 15.00000000000006040 ) ) ;
#1317 = VERTEX_POINT ( 'NONE', #16413 ) ;
#1318 = CARTESIAN_POINT ( 'NONE',  ( -68.99615306438070661, 124.5321250381302463, 15.00000000000006928 ) ) ;
#1319 = DIRECTION ( 'NONE',  ( 0.000000000000000000, 0.000000000000000000, 1.000000000000000000 ) ) ;
#1320 = CARTESIAN_POINT ( 'NONE',  ( -53.97067643794850511, 72.12145385653101926, -15.00000000000001421 ) ) ;
#1321 = ORIENTED_EDGE ( 'NONE', *, *, #5948, .T. ) ;
#1322 = LINE ( 'NONE', #4025, #1514 ) ;
#1323 = DIRECTION ( 'NONE',  ( -1.000000000000000000, 0.000000000000000000, 0.000000000000000000 ) ) ;
#1324 = FILL_AREA_STYLE_COLOUR ( '', #12435 ) ;
#1325 = LINE ( 'NONE', #9738, #8125 ) ;
#1326 = EDGE_LOOP ( 'NONE', ( #17659, #2695, #11593, #11689 ) ) ;
#1327 = AXIS2_PLACEMENT_3D ( 'NONE', #4551, #10267, #13174 ) ;
#1328 = VECTOR ( 'NONE', #6888, 1000.000000000000000 ) ;
#1329 = AXIS2_PLACEMENT_3D ( 'NONE', #12687, #9772, #2750 ) ;
#1330 = CARTESIAN_POINT ( 'NONE',  ( -68.99615306438077766, 123.9172691816626610, 15.00000000000006928 ) ) ;
#1331 = ORIENTED_EDGE ( 'NONE', *, *, #3219, .F. ) ;
#1332 = DIRECTION ( 'NONE',  ( 0.000000000000000000, -5.551115123125748189E-17, -1.000000000000000000 ) ) ;
#1333 = CARTESIAN_POINT ( 'NONE',  ( -71.24615306438076345, 119.0678727652292253, -15.00000000000001421 ) ) ;
#1334 = ORIENTED_EDGE ( 'NONE', *, *, #13295, .F. ) ;
#1335 = ORIENTED_EDGE ( 'NONE', *, *, #1955, .T. ) ;
#1336 = ORIENTED_EDGE ( 'NONE', *, *, #11789, .F. ) ;
#1337 = AXIS2_PLACEMENT_3D ( 'NONE', #5488, #5388, #2600 ) ;
#1338 = AXIS2_PLACEMENT_3D ( 'NONE', #3757, #8048, #13769 ) ;
#1339 = DIRECTION ( 'NONE',  ( 0.000000000000000000, 1.000000000000000000, 0.000000000000000000 ) ) ;
#1340 = CARTESIAN_POINT ( 'NONE',  ( 0.000000000000000000, -5.629165124598954684, 3.250000000000013323 ) ) ;
#1341 = DIRECTION ( 'NONE',  ( -1.000000000000000000, 0.000000000000000000, 0.000000000000000000 ) ) ;
#1342 = ADVANCED_FACE ( 'NONE', ( #13350 ), #525, .T. ) ;
#1343 = LINE ( 'NONE', #5627, #9553 ) ;
#1344 = DIRECTION ( 'NONE',  ( -0.000000000000000000, 0.000000000000000000, -1.000000000000000000 ) ) ;
#1345 = VERTEX_POINT ( 'NONE', #6127 ) ;
#1346 = CARTESIAN_POINT ( 'NONE',  ( -68.99615306438086293, 93.11619853813030545, -167.1454815528550739 ) ) ;
#1348 = ADVANCED_FACE ( 'NONE', ( #3426 ), #11941, .F. ) ;
#1347 = EDGE_LOOP ( 'NONE', ( #13122, #1894, #1210, #14682 ) ) ;
#1349 = LINE ( 'NONE', #7056, #7856 ) ;
#1350 = DIRECTION ( 'NONE',  ( 0.9396926207859145341, 0.3420201433256520596, -1.086737899652996918E-16 ) ) ;
#1351 = ORIENTED_EDGE ( 'NONE', *, *, #2145, .T. ) ;
#1352 = AXIS2_PLACEMENT_3D ( 'NONE', #4171, #12879, #17171 ) ;
#1353 = VECTOR ( 'NONE', #15756, 1000.000000000000000 ) ;
#1354 = CARTESIAN_POINT ( 'NONE',  ( -76.06514409945376087, 73.26749283226919829, 102.5000000000000000 ) ) ;
#1356 = ORIENTED_EDGE ( 'NONE', *, *, #11337, .F. ) ;
#1355 = VECTOR ( 'NONE', #4745, 1000.000000000000000 ) ;
#1357 = VERTEX_POINT ( 'NONE', #12218 ) ;
#1358 = CIRCLE ( 'NONE', #13587, 4.599999999999999645 ) ;
#1359 = CARTESIAN_POINT ( 'NONE',  ( -71.24615306438113294, 16.28418605456381130, -15.00000000000001421 ) ) ;
#1360 = CARTESIAN_POINT ( 'NONE',  ( 5.233202738124664855, -46.83756720124469553, -57.00000000000000000 ) ) ;
#1361 = VECTOR ( 'NONE', #3702, 1000.000000000000000 ) ;
#1362 = ORIENTED_EDGE ( 'NONE', *, *, #12939, .F. ) ;
#1363 = ORIENTED_EDGE ( 'NONE', *, *, #8009, .T. ) ;
#1364 = VECTOR ( 'NONE', #13661, 1000.000000000000000 ) ;
#1365 = AXIS2_PLACEMENT_3D ( 'NONE', #4201, #2708, #5314 ) ;
#1366 = LINE ( 'NONE', #15572, #10483 ) ;
#1367 = DIRECTION ( 'NONE',  ( 1.000000000000000000, 0.000000000000000000, 0.000000000000000000 ) ) ;
#1368 = ORIENTED_EDGE ( 'NONE', *, *, #7763, .T. ) ;
#1369 = CARTESIAN_POINT ( 'NONE',  ( -106.3193689061042164, 112.6569076202650450, 97.49999999999998579 ) ) ;
#1370 = FACE_OUTER_BOUND ( 'NONE', #10235, .T. ) ;
#1371 = LINE ( 'NONE', #4348, #2465 ) ;
#1372 = ORIENTED_EDGE ( 'NONE', *, *, #12466, .T. ) ;
#1373 = DIRECTION ( 'NONE',  ( 1.000000000000000000, 0.000000000000000000, 0.000000000000000000 ) ) ;
#1374 = ORIENTED_EDGE ( 'NONE', *, *, #1830, .T. ) ;
#1375 = ADVANCED_FACE ( 'NONE', ( #13438 ), #10361, .T. ) ;
#1376 = EDGE_LOOP ( 'NONE', ( #11061, #102, #5489, #7491 ) ) ;
#1377 = LINE ( 'NONE', #12792, #2573 ) ;
#1378 = VECTOR ( 'NONE', #1756, 1000.000000000000114 ) ;
#1379 = ORIENTED_EDGE ( 'NONE', *, *, #12840, .T. ) ;
#1380 = ORIENTED_EDGE ( 'NONE', *, *, #3456, .T. ) ;
#1381 = EDGE_CURVE ( 'NONE', #14903, #12673, #14655, .T. ) ;
#1382 = CARTESIAN_POINT ( 'NONE',  ( -57.08002265617300708, 84.22855780814606419, 25.00000000000000355 ) ) ;
#1383 = DIRECTION ( 'NONE',  ( -0.000000000000000000, -0.000000000000000000, -1.000000000000000000 ) ) ;
#1384 = ORIENTED_EDGE ( 'NONE', *, *, #15430, .T. ) ;
#1385 = DIRECTION ( 'NONE',  ( -0.000000000000000000, -1.000000000000000000, -0.000000000000000000 ) ) ;
#1386 = CARTESIAN_POINT ( 'NONE',  ( -55.20348911625212907, 74.15281352429526862, 15.00000000000006928 ) ) ;
#1387 = CARTESIAN_POINT ( 'NONE',  ( 44.74549999999999272, 0.000000000000000000, 0.000000000000000000 ) ) ;
#1388 = ORIENTED_EDGE ( 'NONE', *, *, #3398, .T. ) ;
#1389 = DIRECTION ( 'NONE',  ( 0.000000000000000000, 1.000000000000000000, 0.000000000000000000 ) ) ;
#1390 = CARTESIAN_POINT ( 'NONE',  ( -32.10604320681301971, 43.68747662467802684, -31.38471465307124220 ) ) ;
#1391 = CARTESIAN_POINT ( 'NONE',  ( 15.23320273812465864, -15.06249217057395917, 54.10825519012411178 ) ) ;
#1392 = ORIENTED_EDGE ( 'NONE', *, *, #1153, .T. ) ;
#1393 = ADVANCED_FACE ( 'NONE', ( #18167 ), #2448, .T. ) ;
#1394 = ADVANCED_FACE ( 'NONE', ( #16930 ), #4117, .T. ) ;
#1395 = DIRECTION ( 'NONE',  ( -0.000000000000000000, -0.000000000000000000, -1.000000000000000000 ) ) ;
#1396 = LINE ( 'NONE', #14119, #8408 ) ;
#1397 = LINE ( 'NONE', #14298, #14637 ) ;
#1398 = LINE ( 'NONE', #18508, #12882 ) ;
#1399 = VERTEX_POINT ( 'NONE', #10846 ) ;
#1400 = ORIENTED_EDGE ( 'NONE', *, *, #17950, .F. ) ;
#1401 = EDGE_CURVE ( 'NONE', #2087, #827, #2426, .T. ) ;
#1402 = EDGE_CURVE ( 'NONE', #17364, #4210, #4343, .T. ) ;
#1403 = CYLINDRICAL_SURFACE ( 'NONE', #8481, 4.600000000000006750 ) ;
#1404 = ORIENTED_EDGE ( 'NONE', *, *, #16960, .T. ) ;
#1405 = EDGE_CURVE ( 'NONE', #14435, #10632, #13014, .T. ) ;
#1406 = CARTESIAN_POINT ( 'NONE',  ( -68.99615306438109030, 17.10311908166270456, 15.00000000000006928 ) ) ;
#1407 = EDGE_CURVE ( 'NONE', #8420, #15506, #15340, .T. ) ;
#1408 = CARTESIAN_POINT ( 'NONE',  ( -62.15805688404110185, -91.53392936304808813, -41.62626455281442617 ) ) ;
#1409 = ORIENTED_EDGE ( 'NONE', *, *, #12225, .F. ) ;
#1410 = CARTESIAN_POINT ( 'NONE',  ( -67.59262256747319952, 106.9211863004615140, -28.00000000000000355 ) ) ;
#1411 = FACE_OUTER_BOUND ( 'NONE', #8639, .T. ) ;
#1412 = SURFACE_STYLE_USAGE ( .BOTH. , #4392 ) ;
#1413 = DIRECTION ( 'NONE',  ( 1.000000000000000000, 0.000000000000000000, 0.000000000000000000 ) ) ;
#1414 = ORIENTED_EDGE ( 'NONE', *, *, #17886, .T. ) ;
#1415 = EDGE_CURVE ( 'NONE', #7975, #10340, #3847, .T. ) ;
#1416 = LINE ( 'NONE', #18355, #18244 ) ;
#1417 = EDGE_LOOP ( 'NONE', ( #13121, #10077, #10249, #16577 ) ) ;
#1418 = LINE ( 'NONE', #7121, #16123 ) ;
#1419 = CARTESIAN_POINT ( 'NONE',  ( -57.08002265617300708, 84.22855780814606419, 15.00000000000006928 ) ) ;
#1420 = EDGE_LOOP ( 'NONE', ( #3178, #16210, #16979, #14921 ) ) ;
#1421 = ORIENTED_EDGE ( 'NONE', *, *, #16791, .T. ) ;
#1422 = ORIENTED_EDGE ( 'NONE', *, *, #17047, .T. ) ;
#1423 = FACE_OUTER_BOUND ( 'NONE', #1747, .T. ) ;
#1424 = DIRECTION ( 'NONE',  ( -1.000000000000000000, 2.442490654175343758E-14, 1.387778780781445182E-16 ) ) ;
#1425 = EDGE_CURVE ( 'NONE', #15985, #9812, #6533, .T. ) ;
#1426 = CARTESIAN_POINT ( 'NONE',  ( -78.10583824988592028, 83.23774243329727085, 69.95051152545947559 ) ) ;
#1427 = DIRECTION ( 'NONE',  ( 0.000000000000000000, 0.000000000000000000, 1.000000000000000000 ) ) ;
#1428 = CARTESIAN_POINT ( 'NONE',  ( -68.99615306438106188, 23.38630438166269698, 15.00000000000006928 ) ) ;
#1429 = ORIENTED_EDGE ( 'NONE', *, *, #11980, .F. ) ;
#1430 = LINE ( 'NONE', #4140, #6605 ) ;
#1431 = EDGE_LOOP ( 'NONE', ( #9618, #16149, #15476, #8955 ) ) ;
#1432 = LINE ( 'NONE', #1154, #8770 ) ;
#1433 = CARTESIAN_POINT ( 'NONE',  ( -102.5926225674731569, 65.58224449241410525, 20.00000000000000355 ) ) ;
#1434 = EDGE_LOOP ( 'NONE', ( #6050, #2066, #16636, #4642 ) ) ;
#1435 = CARTESIAN_POINT ( 'NONE',  ( -68.99615306438084872, 77.40823528813027110, 15.00000000000006928 ) ) ;
#1436 = ORIENTED_EDGE ( 'NONE', *, *, #18437, .F. ) ;
#1437 = ADVANCED_FACE ( 'NONE', ( #8030 ), #15235, .T. ) ;
#1438 = ORIENTED_EDGE ( 'NONE', *, *, #14205, .T. ) ;
#1439 = CARTESIAN_POINT ( 'NONE',  ( -60.76828531927866095, 74.07097899412299569, -15.00000000000001421 ) ) ;
#1440 =( REPRESENTATION_RELATIONSHIP ('NONE','NONE', #359, #1677 ) REPRESENTATION_RELATIONSHIP_WITH_TRANSFORMATION ( #8367 )SHAPE_REPRESENTATION_RELATIONSHIP( ) );
#1441 = CARTESIAN_POINT ( 'NONE',  ( -57.08002265617300708, 84.22855780814606419, 77.50000000000000000 ) ) ;
#1442 = FACE_OUTER_BOUND ( 'NONE', #9097, .T. ) ;
#1443 = ORIENTED_EDGE ( 'NONE', *, *, #5918, .F. ) ;
#1444 = EDGE_LOOP ( 'NONE', ( #12591, #14406, #8413, #6180 ) ) ;
#1445 = CARTESIAN_POINT ( 'NONE',  ( -1.560979369245516946, 30.36679981511084137, -38.79937448922311205 ) ) ;
#1446 = LINE ( 'NONE', #12590, #11532 ) ;
#1447 = ORIENTED_EDGE ( 'NONE', *, *, #1173, .T. ) ;
#1448 = AXIS2_PLACEMENT_3D ( 'NONE', #16760, #3769, #10887 ) ;
#1449 = LINE ( 'NONE', #15934, #17350 ) ;
#1450 = CARTESIAN_POINT ( 'NONE',  ( -57.08002265617300708, 84.22855780814606419, -167.1454815528550739 ) ) ;
#1451 = DIRECTION ( 'NONE',  ( 0.000000000000000000, 0.000000000000000000, 1.000000000000000000 ) ) ;
#1452 = ORIENTED_EDGE ( 'NONE', *, *, #344, .T. ) ;
#1453 = LINE ( 'NONE', #7252, #16398 ) ;
#1454 = VERTEX_POINT ( 'NONE', #11037 ) ;
#1455 = ORIENTED_EDGE ( 'NONE', *, *, #11815, .T. ) ;
#1456 = EDGE_CURVE ( 'NONE', #996, #10176, #9633, .T. ) ;
#1457 = CARTESIAN_POINT ( 'NONE',  ( -107.5926225674731853, 110.5691553257988460, 26.35917033480641436 ) ) ;
#1458 = ORIENTED_EDGE ( 'NONE', *, *, #17275, .F. ) ;
#1459 = AXIS2_PLACEMENT_3D ( 'NONE', #9644, #6931, #1135 ) ;
#1460 = VERTEX_POINT ( 'NONE', #10275 ) ;
#1461 = DIRECTION ( 'NONE',  ( 0.000000000000000000, 0.000000000000000000, 1.000000000000000000 ) ) ;
#1462 = VERTEX_POINT ( 'NONE', #11325 ) ;
#1463 = DIRECTION ( 'NONE',  ( 0.9396926207859084279, 0.3420201433256686574, -1.086737899652989892E-16 ) ) ;
#1464 = DIRECTION ( 'NONE',  ( 0.000000000000000000, 0.000000000000000000, 1.000000000000000000 ) ) ;
#1465 = DIRECTION ( 'NONE',  ( 0.000000000000000000, 0.000000000000000000, -1.000000000000000000 ) ) ;
#1466 = CARTESIAN_POINT ( 'NONE',  ( 93.45071565215914688, 84.22855780814606419, 62.50000000000001421 ) ) ;
#1467 = ORIENTED_EDGE ( 'NONE', *, *, #13031, .F. ) ;
#1468 = PLANE ( 'NONE',  #7795 ) ;
#1469 = AXIS2_PLACEMENT_3D ( 'NONE', #9795, #9990, #12519 ) ;
#1470 = LINE ( 'NONE', #7366, #10220 ) ;
#1471 = CARTESIAN_POINT ( 'NONE',  ( 8.585741852500916593, 13.02923129865365048, 46.30804433544984988 ) ) ;
#1472 = ORIENTED_EDGE ( 'NONE', *, *, #9755, .T. ) ;
#1473 = DIRECTION ( 'NONE',  ( -5.204170427930409450E-16, 0.000000000000000000, 1.000000000000000000 ) ) ;
#1474 = DIRECTION ( 'NONE',  ( -0.000000000000000000, -0.000000000000000000, -1.000000000000000000 ) ) ;
#1475 = EDGE_CURVE ( 'NONE', #11152, #12417, #4207, .T. ) ;
#1476 = CARTESIAN_POINT ( 'NONE',  ( -52.17393402261416213, 74.59995546124159205, -167.1454815528550739 ) ) ;
#1477 = CARTESIAN_POINT ( 'NONE',  ( -68.99615306438120399, -1.746436818337276931, -15.00000000000001421 ) ) ;
#1478 = ORIENTED_EDGE ( 'NONE', *, *, #12242, .F. ) ;
#1479 = VERTEX_POINT ( 'NONE', #13094 ) ;
#1480 = VECTOR ( 'NONE', #6149, 1000.000000000000000 ) ;
#1481 = DIRECTION ( 'NONE',  ( 1.156482317317869999E-16, 0.000000000000000000, 1.000000000000000000 ) ) ;
#1482 = ORIENTED_EDGE ( 'NONE', *, *, #9753, .F. ) ;
#1483 = ADVANCED_FACE ( 'NONE', ( #1411 ), #5955, .T. ) ;
#1484 = AXIS2_PLACEMENT_3D ( 'NONE', #18009, #16226, #9221 ) ;
#1485 =( NAMED_UNIT ( * ) PLANE_ANGLE_UNIT ( ) SI_UNIT ( $, .RADIAN. ) );
#1486 = DIRECTION ( 'NONE',  ( 0.000000000000000000, 0.000000000000000000, 1.000000000000000000 ) ) ;
#1487 = CARTESIAN_POINT ( 'NONE',  ( -71.24615306438076345, 119.9567435045637609, -167.1454815528550739 ) ) ;
#1488 = ORIENTED_EDGE ( 'NONE', *, *, #12791, .T. ) ;
#1489 = DIRECTION ( 'NONE',  ( -1.000000000000000000, 0.000000000000000000, 0.000000000000000000 ) ) ;
#1490 = CARTESIAN_POINT ( 'NONE',  ( -68.99615306438094819, 54.80223088166269463, -15.00000000000001421 ) ) ;
#1491 = CARTESIAN_POINT ( 'NONE',  ( -68.99615306438077766, 115.1073470881302541, -167.1454815528550739 ) ) ;
#1492 = EDGE_LOOP ( 'NONE', ( #3530, #10028, #18416, #8612 ) ) ;
#1493 = CARTESIAN_POINT ( 'NONE',  ( 45.30000000000000426, 1.912636715672988680E-16, 3.445500000000021767 ) ) ;
#1494 = ADVANCED_FACE ( 'NONE', ( #1673 ), #15883, .T. ) ;
#1495 = CARTESIAN_POINT ( 'NONE',  ( -57.08002265617300708, 84.22855780814606419, 92.50000000000000000 ) ) ;
#1497 = EDGE_CURVE ( 'NONE', #2307, #10454, #14495, .T. ) ;
#1496 = AXIS2_PLACEMENT_3D ( 'NONE', #8750, #14455, #1638 ) ;
#1498 = ORIENTED_EDGE ( 'NONE', *, *, #17806, .T. ) ;
#1499 = EDGE_CURVE ( 'NONE', #16011, #4288, #11679, .T. ) ;
#1500 = CARTESIAN_POINT ( 'NONE',  ( -68.99615306438083451, 96.25779118813026969, -15.00000000000001421 ) ) ;
#1501 = VECTOR ( 'NONE', #11263, 999.9999999999998863 ) ;
#1502 = CARTESIAN_POINT ( 'NONE',  ( 15.23320273812466041, -46.83756720124470263, 57.00000000000000000 ) ) ;
#1503 = ORIENTED_EDGE ( 'NONE', *, *, #8170, .T. ) ;
#1504 = ORIENTED_EDGE ( 'NONE', *, *, #7764, .F. ) ;
#1505 = ADVANCED_FACE ( 'NONE', ( #3073 ), #5603, .T. ) ;
#1506 = EDGE_CURVE ( 'NONE', #11023, #8947, #5547, .T. ) ;
#1507 = EDGE_CURVE ( 'NONE', #573, #17254, #15800, .T. ) ;
#1508 = CARTESIAN_POINT ( 'NONE',  ( -80.43148536604020649, 78.95224028009165806, 102.5000000000000000 ) ) ;
#1509 = LINE ( 'NONE', #8625, #8478 ) ;
#1510 = AXIS2_PLACEMENT_3D ( 'NONE', #11710, #6160, #4861 ) ;
#1511 = CARTESIAN_POINT ( 'NONE',  ( -68.99615306438080609, 108.8241617881302545, -15.00000000000001421 ) ) ;
#1512 = EDGE_CURVE ( 'NONE', #425, #18243, #17284, .T. ) ;
#1513 = CYLINDRICAL_SURFACE ( 'NONE', #8051, 4.599999999999992539 ) ;
#1514 = VECTOR ( 'NONE', #5414, 999.9999999999998863 ) ;
#1515 = DIRECTION ( 'NONE',  ( 1.000000000000000000, 0.000000000000000000, 0.000000000000000000 ) ) ;
#1516 = VECTOR ( 'NONE', #2698, 1000.000000000000000 ) ;
#1517 = ORIENTED_EDGE ( 'NONE', *, *, #12616, .T. ) ;
#1518 = CARTESIAN_POINT ( 'NONE',  ( -98.90286936182226896, -96.08423613455721579, -10.65431531532588494 ) ) ;
#1519 = VERTEX_POINT ( 'NONE', #12751 ) ;
#1520 = CARTESIAN_POINT ( 'NONE',  ( -80.06812138002696599, -91.24992890033500714, 40.65007677557128574 ) ) ;
#1521 = DIRECTION ( 'NONE',  ( -1.558623840612994987E-16, -1.000000000000000000, 0.000000000000000000 ) ) ;
#1522 = ORIENTED_EDGE ( 'NONE', *, *, #8000, .F. ) ;
#1523 = AXIS2_PLACEMENT_3D ( 'NONE', #13994, #2279, #16596 ) ;
#1524 = DIRECTION ( 'NONE',  ( 0.000000000000000000, 0.000000000000000000, 1.000000000000000000 ) ) ;
#1525 = EDGE_CURVE ( 'NONE', #10995, #13256, #5846, .T. ) ;
#1526 = VERTEX_POINT ( 'NONE', #2815 ) ;
#1527 = VECTOR ( 'NONE', #9452, 1000.000000000000000 ) ;
#1528 = ADVANCED_FACE ( 'NONE', ( #17112 ), #14234, .T. ) ;
#1529 = CIRCLE ( 'NONE', #11967, 4.599999999999999645 ) ;
#1530 = CIRCLE ( 'NONE', #16093, 20.99999999999998934 ) ;
#1531 = ORIENTED_EDGE ( 'NONE', *, *, #11525, .T. ) ;
#1532 = DIRECTION ( 'NONE',  ( -5.204170427930409450E-16, 0.000000000000000000, 1.000000000000000000 ) ) ;
#1533 = DIRECTION ( 'NONE',  ( 1.000000000000000000, 0.000000000000000000, 0.000000000000000000 ) ) ;
#1534 = DIRECTION ( 'NONE',  ( 0.3420201433256686574, 0.9396926207859084279, -0.000000000000000000 ) ) ;
#1535 = VERTEX_POINT ( 'NONE', #4302 ) ;
#1536 = AXIS2_PLACEMENT_3D ( 'NONE', #16378, #3567, #17511 ) ;
#1537 = ORIENTED_EDGE ( 'NONE', *, *, #14930, .T. ) ;
#1538 = DIRECTION ( 'NONE',  ( 0.9396926207859148672, 0.3420201433256507273, 0.000000000000000000 ) ) ;
#1539 = CYLINDRICAL_SURFACE ( 'NONE', #2742, 12.50000000000001776 ) ;
#1540 = DIRECTION ( 'NONE',  ( -1.000000000000000000, 0.000000000000000000, 0.000000000000000000 ) ) ;
#1541 = AXIS2_PLACEMENT_3D ( 'NONE', #17995, #9123, #14899 ) ;
#1542 = ORIENTED_EDGE ( 'NONE', *, *, #14644, .T. ) ;
#1543 = LINE ( 'NONE', #2766, #3559 ) ;
#1544 = ORIENTED_EDGE ( 'NONE', *, *, #15274, .F. ) ;
#1545 = EDGE_LOOP ( 'NONE', ( #2115, #5640, #5377, #8327 ) ) ;
#1546 = AXIS2_PLACEMENT_3D ( 'NONE', #7135, #17137, #4325 ) ;
#1547 = ORIENTED_EDGE ( 'NONE', *, *, #16169, .F. ) ;
#1548 = AXIS2_PLACEMENT_3D ( 'NONE', #12923, #5789, #3250 ) ;
#1549 = CIRCLE ( 'NONE', #5112, 4.000000000000003553 ) ;
#1550 = ORIENTED_EDGE ( 'NONE', *, *, #13051, .T. ) ;
#1551 = DIRECTION ( 'NONE',  ( 0.000000000000000000, 0.000000000000000000, -1.000000000000000000 ) ) ;
#1552 = ORIENTED_EDGE ( 'NONE', *, *, #7421, .T. ) ;
#1553 = CARTESIAN_POINT ( 'NONE',  ( -68.99615306438070661, 140.2400882881302948, -15.00000000000001421 ) ) ;
#1554 = DIRECTION ( 'NONE',  ( -0.000000000000000000, -0.000000000000000000, 1.000000000000000000 ) ) ;
#1555 = DIRECTION ( 'NONE',  ( 0.000000000000000000, 0.000000000000000000, 1.000000000000000000 ) ) ;
#1556 = EDGE_LOOP ( 'NONE', ( #15169, #11479, #6546, #10377 ) ) ;
#1557 = PRODUCT_DEFINITION ( 'UNKNOWN', '', #10279, #3650 ) ;
#1558 = AXIS2_PLACEMENT_3D ( 'NONE', #9037, #14726, #7811 ) ;
#1559 = CARTESIAN_POINT ( 'NONE',  ( -68.99615306438072082, 127.0588618316627105, -167.1454815528550739 ) ) ;
#1560 = DIRECTION ( 'NONE',  ( 0.000000000000000000, 0.000000000000000000, 1.000000000000000000 ) ) ;
#1561 = PLANE ( 'NONE',  #12933 ) ;
#1562 = VERTEX_POINT ( 'NONE', #11595 ) ;
#1563 = EDGE_CURVE ( 'NONE', #11670, #2929, #1579, .T. ) ;
#1564 = VECTOR ( 'NONE', #9130, 1000.000000000000000 ) ;
#1565 = VECTOR ( 'NONE', #8531, 1000.000000000000000 ) ;
#1566 = CARTESIAN_POINT ( 'NONE',  ( -68.99615306438094819, 70.51019413166270056, -15.00000000000001421 ) ) ;
#1567 = DIRECTION ( 'NONE',  ( 0.000000000000000000, 0.000000000000000000, 1.000000000000000000 ) ) ;
#1568 = ORIENTED_EDGE ( 'NONE', *, *, #6498, .F. ) ;
#1569 = ORIENTED_EDGE ( 'NONE', *, *, #3664, .F. ) ;
#1570 = AXIS2_PLACEMENT_3D ( 'NONE', #5555, #6963, #6776 ) ;
#1571 = CARTESIAN_POINT ( 'NONE',  ( -65.06546592763082515, -91.08423613455721579, -45.05044770573174873 ) ) ;
#1572 = VECTOR ( 'NONE', #9277, 1000.000000000000000 ) ;
#1573 = VECTOR ( 'NONE', #11269, 1000.000000000000000 ) ;
#1574 = DIRECTION ( 'NONE',  ( 0.000000000000000000, 0.000000000000000000, 1.000000000000000000 ) ) ;
#1575 = CARTESIAN_POINT ( 'NONE',  ( -107.5926225674732137, 117.8748711238780373, 25.00000000000000000 ) ) ;
#1576 = CARTESIAN_POINT ( 'NONE',  ( -71.24615306438106188, 37.38646386522923137, -15.00000000000001421 ) ) ;
#1577 = ORIENTED_EDGE ( 'NONE', *, *, #16595, .T. ) ;
#1578 = DIRECTION ( 'NONE',  ( -1.224646799147353207E-16, 1.000000000000000000, 0.000000000000000000 ) ) ;
#1579 = LINE ( 'NONE', #5875, #12744 ) ;
#1580 = DIRECTION ( 'NONE',  ( 0.000000000000000000, 5.551115123125747573E-17, 1.000000000000000000 ) ) ;
#1581 = PLANE ( 'NONE',  #6951 ) ;
#1582 = ORIENTED_EDGE ( 'NONE', *, *, #9376, .T. ) ;
#1583 = CARTESIAN_POINT ( 'NONE',  ( -36.05803997522690452, 85.21341043856776309, 69.93917279341883386 ) ) ;
#1584 = AXIS2_PLACEMENT_3D ( 'NONE', #10488, #5054, #17786 ) ;
#1585 = FACE_OUTER_BOUND ( 'NONE', #1876, .T. ) ;
#1586 = ORIENTED_EDGE ( 'NONE', *, *, #10900, .F. ) ;
#1587 = ADVANCED_FACE ( 'NONE', ( #2907 ), #8693, .T. ) ;
#1588 = VECTOR ( 'NONE', #2520, 1000.000000000000000 ) ;
#1589 = CYLINDRICAL_SURFACE ( 'NONE', #16728, 7.168074330099291736 ) ;
#1590 = AXIS2_PLACEMENT_3D ( 'NONE', #6597, #3600, #13810 ) ;
#1591 = DIRECTION ( 'NONE',  ( 0.000000000000000000, 1.000000000000000000, 0.000000000000000000 ) ) ;
#1592 = ORIENTED_EDGE ( 'NONE', *, *, #362, .T. ) ;
#1593 = CIRCLE ( 'NONE', #3977, 9.999999999999994671 ) ;
#1594 = EDGE_LOOP ( 'NONE', ( #5775, #9382, #2860, #1057 ) ) ;
#1595 = VECTOR ( 'NONE', #6503, 1000.000000000000000 ) ;
#1596 = ORIENTED_EDGE ( 'NONE', *, *, #8148, .T. ) ;
#1597 = LINE ( 'NONE', #17127, #15379 ) ;
#1598 = DIRECTION ( 'NONE',  ( -5.204170427930409450E-16, 0.000000000000000000, 1.000000000000000000 ) ) ;
#1599 = EDGE_CURVE ( 'NONE', #11975, #10530, #91, .T. ) ;
#1600 = CARTESIAN_POINT ( 'NONE',  ( -67.44681693414594292, 91.21279551874751235, -167.1454815528550739 ) ) ;
#1601 = EDGE_CURVE ( 'NONE', #12783, #14981, #4357, .T. ) ;
#1602 = CARTESIAN_POINT ( 'NONE',  ( 103.5381772159376084, 0.000000000000000000, 36.00000000000000711 ) ) ;
#1603 = VECTOR ( 'NONE', #6733, 1000.000000000000000 ) ;
#1604 = AXIS2_PLACEMENT_3D ( 'NONE', #7164, #17432, #58 ) ;
#1605 = FACE_OUTER_BOUND ( 'NONE', #1444, .T. ) ;
#1606 = ORIENTED_EDGE ( 'NONE', *, *, #11097, .F. ) ;
#1607 = CARTESIAN_POINT ( 'NONE',  ( -55.10846673861666289, 96.57209730311868157, -15.00000000000001421 ) ) ;
#1608 = ORIENTED_EDGE ( 'NONE', *, *, #9877, .T. ) ;
#1609 = LINE ( 'NONE', #17494, #12670 ) ;
#1610 = LINE ( 'NONE', #10211, #4762 ) ;
#1611 = ORIENTED_EDGE ( 'NONE', *, *, #16336, .F. ) ;
#1612 = EDGE_CURVE ( 'NONE', #1562, #14366, #7338, .T. ) ;
#1613 = ADVANCED_FACE ( 'NONE', ( #17468 ), #13270, .T. ) ;
#1614 = FACE_OUTER_BOUND ( 'NONE', #6932, .T. ) ;
#1615 = CARTESIAN_POINT ( 'NONE',  ( -111.0396820472913220, -91.18731257919070288, -9.610190611755886181 ) ) ;
#1616 = VERTEX_POINT ( 'NONE', #8880 ) ;
#1617 = AXIS2_PLACEMENT_3D ( 'NONE', #17088, #18415, #11303 ) ;
#1618 = AXIS2_PLACEMENT_3D ( 'NONE', #1086, #2575, #8275 ) ;
#1619 = ORIENTED_EDGE ( 'NONE', *, *, #795, .T. ) ;
#1620 = ADVANCED_FACE ( 'NONE', ( #450 ), #11946, .T. ) ;
#1621 = CARTESIAN_POINT ( 'NONE',  ( -68.99615306438089135, 86.21815738166266385, -15.00000000000001421 ) ) ;
#1622 = EDGE_CURVE ( 'NONE', #288, #455, #4830, .T. ) ;
#1623 = CARTESIAN_POINT ( 'NONE',  ( -57.08002265617300708, 84.22855780814606419, -167.1454815528550739 ) ) ;
#1624 = LINE ( 'NONE', #7334, #18309 ) ;
#1625 = PRESENTATION_LAYER_ASSIGNMENT (  '', '', ( #1046 ) ) ;
#1626 = ORIENTED_EDGE ( 'NONE', *, *, #3642, .T. ) ;
#1627 = EDGE_CURVE ( 'NONE', #2025, #11979, #10549, .T. ) ;
#1628 = ADVANCED_FACE ( 'NONE', ( #6320 ), #16244, .F. ) ;
#1629 = EDGE_LOOP ( 'NONE', ( #8679, #16373, #14384, #17205 ) ) ;
#1630 = VECTOR ( 'NONE', #11480, 1000.000000000000000 ) ;
#1631 = DIRECTION ( 'NONE',  ( -1.000000000000000000, -0.000000000000000000, -0.000000000000000000 ) ) ;
#1632 = DIRECTION ( 'NONE',  ( 0.000000000000000000, 1.000000000000000000, 0.000000000000000000 ) ) ;
#1633 = FACE_OUTER_BOUND ( 'NONE', #16999, .T. ) ;
#1634 = DIRECTION ( 'NONE',  ( -1.982541115402065702E-15, 0.000000000000000000, -1.000000000000000000 ) ) ;
#1635 = VECTOR ( 'NONE', #9124, 1000.000000000000000 ) ;
#1636 = VERTEX_POINT ( 'NONE', #10725 ) ;
#1637 = VECTOR ( 'NONE', #1965, 1000.000000000000000 ) ;
#1638 = DIRECTION ( 'NONE',  ( 1.000000000000000000, 0.000000000000000000, 0.000000000000000000 ) ) ;
#1639 = EDGE_LOOP ( 'NONE', ( #3526, #4049 ) ) ;
#1640 = EDGE_CURVE ( 'NONE', #3309, #2052, #3169, .T. ) ;
#1641 = ORIENTED_EDGE ( 'NONE', *, *, #14385, .T. ) ;
#1642 = VECTOR ( 'NONE', #3579, 1000.000000000000000 ) ;
#1643 = ORIENTED_EDGE ( 'NONE', *, *, #15148, .T. ) ;
#1644 = VECTOR ( 'NONE', #9718, 1000.000000000000000 ) ;
#1645 = AXIS2_PLACEMENT_3D ( 'NONE', #15236, #839, #5130 ) ;
#1646 = DIRECTION ( 'NONE',  ( -1.000000000000000000, 0.000000000000000000, 0.000000000000000000 ) ) ;
#1647 = CARTESIAN_POINT ( 'NONE',  ( -76.37409655828275845, -96.08423613455721579, 28.18308811886536347 ) ) ;
#1648 = DIRECTION ( 'NONE',  ( 0.000000000000000000, 1.000000000000000000, 0.000000000000000000 ) ) ;
#1649 = LINE ( 'NONE', #13075, #8345 ) ;
#1650 = CARTESIAN_POINT ( 'NONE',  ( -68.99615306438094819, 51.66063823166267355, 15.00000000000006928 ) ) ;
#1651 = DIRECTION ( 'NONE',  ( 0.000000000000000000, 0.000000000000000000, -1.000000000000000000 ) ) ;
#1652 = ORIENTED_EDGE ( 'NONE', *, *, #11348, .T. ) ;
#1653 = DIRECTION ( 'NONE',  ( 1.000000000000000000, 0.000000000000000000, 0.000000000000000000 ) ) ;
#1654 = CARTESIAN_POINT ( 'NONE',  ( -71.24615306438109030, 31.10327856522923540, -167.1454815528550739 ) ) ;
#1655 = DIRECTION ( 'NONE',  ( 1.000000000000000000, 2.062304371594500247E-16, 0.000000000000000000 ) ) ;
#1656 = VERTEX_POINT ( 'NONE', #12146 ) ;
#1657 = VECTOR ( 'NONE', #15980, 1000.000000000000000 ) ;
#1658 = AXIS2_PLACEMENT_3D ( 'NONE', #8609, #14313, #12919 ) ;
#1659 = CARTESIAN_POINT ( 'NONE',  ( -57.08002265617300708, 84.22855780814606419, -167.1454815528550739 ) ) ;
#1660 = FACE_OUTER_BOUND ( 'NONE', #4429, .T. ) ;
#1661 = VERTEX_POINT ( 'NONE', #14573 ) ;
#1662 = VERTEX_POINT ( 'NONE', #4932 ) ;
#1663 = FACE_OUTER_BOUND ( 'NONE', #16501, .T. ) ;
#1664 = ADVANCED_FACE ( 'NONE', ( #3518 ), #9151, .T. ) ;
#1665 = CIRCLE ( 'NONE', #7895, 3.999999999999996447 ) ;
#1666 = CARTESIAN_POINT ( 'NONE',  ( 0.000000000000000000, 0.000000000000000000, 0.000000000000000000 ) ) ;
#1667 = AXIS2_PLACEMENT_3D ( 'NONE', #16475, #7969, #17976 ) ;
#1668 =( NAMED_UNIT ( * ) PLANE_ANGLE_UNIT ( ) SI_UNIT ( $, .RADIAN. ) );
#1669 = CARTESIAN_POINT ( 'NONE',  ( -60.62932119839002354, 94.43552448259767118, -15.00000000000001421 ) ) ;
#1670 = PLANE ( 'NONE',  #4317 ) ;
#1671 = ORIENTED_EDGE ( 'NONE', *, *, #12257, .F. ) ;
#1672 = DIRECTION ( 'NONE',  ( -1.000000000000000000, 0.000000000000000000, 0.000000000000000000 ) ) ;
#1673 = FACE_OUTER_BOUND ( 'NONE', #10403, .T. ) ;
#1674 = CARTESIAN_POINT ( 'NONE',  ( -71.24615306438080609, 103.3599095152292193, -167.1454815528550739 ) ) ;
#1675 = LINE ( 'NONE', #15728, #4539 ) ;
#1676 = CARTESIAN_POINT ( 'NONE',  ( -37.41836177203395408, 91.72869609463791107, 62.99211610237011172 ) ) ;
#1677 = SHAPE_REPRESENTATION ( 'Plastic-Ended Handle', ( #16217 ), #12057 ) ;
#1678 = LINE ( 'NONE', #15889, #13452 ) ;
#1679 = ORIENTED_EDGE ( 'NONE', *, *, #6527, .F. ) ;
#1680 = DIRECTION ( 'NONE',  ( -0.9396926207859008784, 0.3420201433256891965, -4.890320548438409462E-16 ) ) ;
#1681 = CARTESIAN_POINT ( 'NONE',  ( -68.99615306438077766, 114.4924912316626688, 15.00000000000006928 ) ) ;
#1682 = ORIENTED_EDGE ( 'NONE', *, *, #17517, .T. ) ;
#1683 = ADVANCED_FACE ( 'NONE', ( #16145 ), #6424, .T. ) ;
#1684 = ORIENTED_EDGE ( 'NONE', *, *, #18102, .F. ) ;
#1685 = ORIENTED_EDGE ( 'NONE', *, *, #6372, .F. ) ;
#1686 = DIRECTION ( 'NONE',  ( 0.000000000000000000, 0.000000000000000000, 1.000000000000000000 ) ) ;
#1687 = CARTESIAN_POINT ( 'NONE',  ( -68.99615306438083451, 102.5409764881302692, -167.1454815528550739 ) ) ;
#1688 = DIRECTION ( 'NONE',  ( 0.000000000000000000, 1.000000000000000000, 0.000000000000000000 ) ) ;
#1689 = EDGE_CURVE ( 'NONE', #11390, #9243, #16057, .T. ) ;
#1690 = DIRECTION ( 'NONE',  ( -1.000000000000000000, 0.000000000000000000, 0.000000000000000000 ) ) ;
#1691 = LINE ( 'NONE', #14251, #2758 ) ;
#1692 = ORIENTED_EDGE ( 'NONE', *, *, #9138, .F. ) ;
#1693 = FACE_OUTER_BOUND ( 'NONE', #14514, .T. ) ;
#1694 = DIRECTION ( 'NONE',  ( -1.000000000000000000, -2.062304371594500740E-16, -0.000000000000000000 ) ) ;
#1695 = CARTESIAN_POINT ( 'NONE',  ( -66.39923980726636898, 75.89776002577445979, -15.00000000000001421 ) ) ;
#1696 = EDGE_LOOP ( 'NONE', ( #13023, #4065, #7411, #10027 ) ) ;
#1697 = CARTESIAN_POINT ( 'NONE',  ( -68.99615306438106188, 23.38630438166269698, -167.1454815528550739 ) ) ;
#1698 = CARTESIAN_POINT ( 'NONE',  ( -56.16856596726385220, 74.02016676429185793, -167.1454815528550739 ) ) ;
#1699 = ORIENTED_EDGE ( 'NONE', *, *, #16467, .T. ) ;
#1700 = ADVANCED_FACE ( 'NONE', ( #8966 ), #3247, .F. ) ;
#1701 = ORIENTED_EDGE ( 'NONE', *, *, #11701, .F. ) ;
#1702 = LINE ( 'NONE', #16087, #17458 ) ;
#1703 = CARTESIAN_POINT ( 'NONE',  ( -212.2032458117903104, 84.22855780814606419, 72.88004356723772048 ) ) ;
#1704 = CARTESIAN_POINT ( 'NONE',  ( -68.99615306438117557, 2.010011688130281193, 15.00000000000006928 ) ) ;
#1705 = EDGE_CURVE ( 'NONE', #9559, #15506, #7461, .T. ) ;
#1706 = ORIENTED_EDGE ( 'NONE', *, *, #8132, .F. ) ;
#1707 = EDGE_CURVE ( 'NONE', #14706, #2059, #13179, .T. ) ;
#1708 = VERTEX_POINT ( 'NONE', #13355 ) ;
#1709 = CARTESIAN_POINT ( 'NONE',  ( -68.99615306438073503, 105.6825691381302761, 15.00000000000006928 ) ) ;
#1710 = ADVANCED_FACE ( 'NONE', ( #355 ), #6044, .F. ) ;
#1711 = PLANE ( 'NONE',  #44 ) ;
#1712 = DIRECTION ( 'NONE',  ( 0.000000000000000000, 0.000000000000000000, 1.000000000000000000 ) ) ;
#1713 = FACE_OUTER_BOUND ( 'NONE', #7475, .T. ) ;
#1714 = ORIENTED_EDGE ( 'NONE', *, *, #10903, .T. ) ;
#1715 = PLANE ( 'NONE',  #2686 ) ;
#1716 = VERTEX_POINT ( 'NONE', #1851 ) ;
#1717 = EDGE_CURVE ( 'NONE', #401, #16431, #11237, .T. ) ;
#1718 = ORIENTED_EDGE ( 'NONE', *, *, #903, .F. ) ;
#1719 = ADVANCED_FACE ( 'NONE', ( #9711 ), #5392, .T. ) ;
#1720 = EDGE_CURVE ( 'NONE', #10424, #16418, #14506, .T. ) ;
#1721 = EDGE_CURVE ( 'NONE', #7210, #14794, #5491, .T. ) ;
#1722 = ORIENTED_EDGE ( 'NONE', *, *, #15781, .F. ) ;
#1723 =( NAMED_UNIT ( * ) PLANE_ANGLE_UNIT ( ) SI_UNIT ( $, .RADIAN. ) );
#1724 = LINE ( 'NONE', #7429, #16218 ) ;
#1725 = ADVANCED_FACE ( 'NONE', ( #15419 ), #15211, .T. ) ;
#1726 = EDGE_LOOP ( 'NONE', ( #5270, #13430, #4448, #13516 ) ) ;
#1727 = EDGE_CURVE ( 'NONE', #5292, #11248, #17479, .T. ) ;
#1728 = ADVANCED_FACE ( 'NONE', ( #7932 ), #14014, .T. ) ;
#1729 = CARTESIAN_POINT ( 'NONE',  ( -76.06514409945376087, 73.26749283226919829, 92.50000000000000000 ) ) ;
#1730 = DIRECTION ( 'NONE',  ( -0.9396926207859069846, 0.3420201433256723766, 1.086737899652988166E-16 ) ) ;
#1731 = CARTESIAN_POINT ( 'NONE',  ( -71.24615306438076345, 132.5231141045637457, 15.00000000000006928 ) ) ;
#1732 = DIRECTION ( 'NONE',  ( -1.000000000000000000, 0.000000000000000000, -3.223492141267075737E-15 ) ) ;
#1733 = ORIENTED_EDGE ( 'NONE', *, *, #16224, .T. ) ;
#1734 = PLANE ( 'NONE',  #3910 ) ;
#1735 = CYLINDRICAL_SURFACE ( 'NONE', #9620, 9.197489084949710403 ) ;
#1736 = CARTESIAN_POINT ( 'NONE',  ( -57.08002265617300708, 84.22855780814606419, -15.00000000000001421 ) ) ;
#1737 = ORIENTED_EDGE ( 'NONE', *, *, #5821, .T. ) ;
#1738 = CARTESIAN_POINT ( 'NONE',  ( -68.99615306438109030, 17.71797493813028268, -167.1454815528550739 ) ) ;
#1739 = CIRCLE ( 'NONE', #11889, 4.599999999999992539 ) ;
#1740 = PLANE ( 'NONE',  #13721 ) ;
#1741 = ORIENTED_EDGE ( 'NONE', *, *, #11659, .T. ) ;
#1742 = ADVANCED_FACE ( 'NONE', ( #6607 ), #6898, .T. ) ;
#1743 = EDGE_CURVE ( 'NONE', #4878, #13376, #18026, .T. ) ;
#1744 = EDGE_LOOP ( 'NONE', ( #2481, #4950, #13639, #5885 ) ) ;
#1745 = VERTEX_POINT ( 'NONE', #18129 ) ;
#1746 = DIRECTION ( 'NONE',  ( -0.000000000000000000, -1.000000000000000000, -0.000000000000000000 ) ) ;
#1747 = EDGE_LOOP ( 'NONE', ( #12529, #685, #8352, #12835 ) ) ;
#1748 = DIRECTION ( 'NONE',  ( 1.000000000000000000, 0.000000000000000000, 0.000000000000000000 ) ) ;
#1749 = CARTESIAN_POINT ( 'NONE',  ( -66.21742401348355145, 112.1398742197459910, -27.07089588484168985 ) ) ;
#1750 = LINE ( 'NONE', #17362, #12354 ) ;
#1751 = VECTOR ( 'NONE', #2825, 1000.000000000000000 ) ;
#1752 = CARTESIAN_POINT ( 'NONE',  ( 93.45071565215914688, 84.22855780814606419, 74.79357405616491405 ) ) ;
#1753 = EDGE_LOOP ( 'NONE', ( #14207, #862, #15105, #13118, #7710, #9924 ) ) ;
#1754 = CARTESIAN_POINT ( 'NONE',  ( -59.37303238940180705, 94.21775734381046163, -167.1454815528550739 ) ) ;
#1755 = CARTESIAN_POINT ( 'NONE',  ( -64.09025127992788384, 50.58224449241410525, 35.00000000000000000 ) ) ;
#1756 = DIRECTION ( 'NONE',  ( -0.9396926207859171987, 0.3420201433256444545, 1.086737899652999999E-16 ) ) ;
#1757 = CARTESIAN_POINT ( 'NONE',  ( -1.219346279219927580E-14, 0.6351314446024779459, 6.499999999999983125 ) ) ;
#1758 = CARTESIAN_POINT ( 'NONE',  ( -36.37230694946377696, 87.99602245404176415, 55.99668402450813431 ) ) ;
#1759 = CARTESIAN_POINT ( 'NONE',  ( -71.24615306438076345, 125.3510580652292248, 15.00000000000006928 ) ) ;
#1760 = ORIENTED_EDGE ( 'NONE', *, *, #18165, .T. ) ;
#1761 = B_SPLINE_CURVE_WITH_KNOTS ( 'NONE', 3,
 ( #11746, #7528, #4531, #3226, #11921, #424 ),
 .UNSPECIFIED., .F., .F.,
 ( 4, 2, 4 ),
 ( 0.006874058789394440171, 0.008773169699889987044, 0.01067228061038553305 ),
 .UNSPECIFIED. ) ;
#1762 = EDGE_CURVE ( 'NONE', #12741, #9327, #15124, .T. ) ;
#1763 = DIRECTION ( 'NONE',  ( 1.000000000000000000, 2.062304371594500494E-16, 0.000000000000000000 ) ) ;
#1764 = CARTESIAN_POINT ( 'NONE',  ( 5.299999999999998934, 3.752776749732559924, -6.500000000000061284 ) ) ;
#1765 = ORIENTED_EDGE ( 'NONE', *, *, #15575, .T. ) ;
#1766 = AXIS2_PLACEMENT_3D ( 'NONE', #11702, #7394, #17033 ) ;
#1767 = ORIENTED_EDGE ( 'NONE', *, *, #6616, .T. ) ;
#1768 = ORIENTED_EDGE ( 'NONE', *, *, #6527, .T. ) ;
#1769 = CARTESIAN_POINT ( 'NONE',  ( -107.5676225674731938, 110.5691553257988460, -30.35917033480641791 ) ) ;
#1770 = CARTESIAN_POINT ( 'NONE',  ( -57.08002265617300708, 84.22855780814606419, -15.00000000000001421 ) ) ;
#1771 = LINE ( 'NONE', #7479, #8037 ) ;
#1772 = LINE ( 'NONE', #1871, #3126 ) ;
#1773 = DIRECTION ( 'NONE',  ( -0.000000000000000000, -0.000000000000000000, -1.000000000000000000 ) ) ;
#1774 = CYLINDRICAL_SURFACE ( 'NONE', #16267, 4.999999999999997335 ) ;
#1775 = LINE ( 'NONE', #1428, #14980 ) ;
#1776 = ORIENTED_EDGE ( 'NONE', *, *, #16329, .F. ) ;
#1777 = AXIS2_PLACEMENT_3D ( 'NONE', #6183, #16658, #11066 ) ;
#1778 = ADVANCED_FACE ( 'NONE', ( #3809 ), #13608, .T. ) ;
#1779 = CARTESIAN_POINT ( 'NONE',  ( -97.59262256747318531, 0.3328663868096687350, -25.00000000000000000 ) ) ;
#1780 = CARTESIAN_POINT ( 'NONE',  ( -79.54423376290981196, -91.42293805878658475, 41.30286037549874578 ) ) ;
#1781 = VECTOR ( 'NONE', #15202, 1000.000000000000000 ) ;
#1782 = DIRECTION ( 'NONE',  ( 0.9396926207859157554, 0.3420201433256481738, 4.890320548438487362E-16 ) ) ;
#1783 = ORIENTED_EDGE ( 'NONE', *, *, #5382, .T. ) ;
#1784 = DIRECTION ( 'NONE',  ( -1.000000000000000000, -0.000000000000000000, -0.000000000000000000 ) ) ;
#1785 = CARTESIAN_POINT ( 'NONE',  ( -46.03642545851251100, 84.22855780814606419, 37.50000000000000000 ) ) ;
#1786 = ORIENTED_EDGE ( 'NONE', *, *, #13989, .T. ) ;
#1787 = VECTOR ( 'NONE', #3639, 1000.000000000000000 ) ;
#1788 = ORIENTED_EDGE ( 'NONE', *, *, #335, .F. ) ;
#1789 = AXIS2_PLACEMENT_3D ( 'NONE', #17035, #4136, #5539 ) ;
#1790 = VECTOR ( 'NONE', #11526, 1000.000000000000114 ) ;
#1791 = DIRECTION ( 'NONE',  ( 0.000000000000000000, 0.000000000000000000, 1.000000000000000000 ) ) ;
#1792 = CARTESIAN_POINT ( 'NONE',  ( 95.45835937779683888, -32.62665103886256190, 7.000000000000010658 ) ) ;
#1793 = CARTESIAN_POINT ( 'NONE',  ( -68.99615306438072082, 133.3420471316626958, 15.00000000000006928 ) ) ;
#1794 = ORIENTED_EDGE ( 'NONE', *, *, #6396, .T. ) ;
#1795 = EDGE_LOOP ( 'NONE', ( #10974, #9798, #1882, #12578 ) ) ;
#1796 = DIRECTION ( 'NONE',  ( 0.3822456275482439270, -0.9240607556975077852, 0.000000000000000000 ) ) ;
#1797 = DIRECTION ( 'NONE',  ( 0.000000000000000000, 1.000000000000000000, 0.000000000000000000 ) ) ;
#1798 = CARTESIAN_POINT ( 'NONE',  ( -68.99615306438106188, 30.28434553813027108, -167.1454815528550739 ) ) ;
#1799 = CIRCLE ( 'NONE', #2107, 10.24900000000001477 ) ;
#1800 = EDGE_CURVE ( 'NONE', #17240, #9888, #2217, .T. ) ;
#1801 = LINE ( 'NONE', #8920, #18007 ) ;
#1802 = ORIENTED_EDGE ( 'NONE', *, *, #13045, .T. ) ;
#1803 = VECTOR ( 'NONE', #8241, 1000.000000000000114 ) ;
#1804 = CARTESIAN_POINT ( 'NONE',  ( -93.54007869656271623, 187.7866419848965052, -167.1454815528550739 ) ) ;
#1805 = ORIENTED_EDGE ( 'NONE', *, *, #15999, .T. ) ;
#1806 = VECTOR ( 'NONE', #12722, 1000.000000000000000 ) ;
#1807 = FACE_OUTER_BOUND ( 'NONE', #3297, .T. ) ;
#1808 = ORIENTED_EDGE ( 'NONE', *, *, #989, .T. ) ;
#1809 = AXIS2_PLACEMENT_3D ( 'NONE', #16405, #17904, #7814 ) ;
#1810 = ADVANCED_FACE ( 'NONE', ( #905 ), #6119, .T. ) ;
#1811 = ORIENTED_EDGE ( 'NONE', *, *, #16462, .T. ) ;
#1812 = VECTOR ( 'NONE', #17999, 1000.000000000000000 ) ;
#1813 = CARTESIAN_POINT ( 'NONE',  ( -63.80603561266293156, 73.69239390902558284, 15.00000000000006928 ) ) ;
#1814 = DIRECTION ( 'NONE',  ( -1.000000000000000000, 0.000000000000000000, 0.000000000000000000 ) ) ;
#1815 = ORIENTED_EDGE ( 'NONE', *, *, #15689, .T. ) ;
#1816 = VECTOR ( 'NONE', #7709, 1000.000000000000000 ) ;
#1817 = VECTOR ( 'NONE', #1554, 1000.000000000000000 ) ;
#1818 = DIRECTION ( 'NONE',  ( 0.000000000000000000, 0.000000000000000000, 1.000000000000000000 ) ) ;
#1819 = FACE_OUTER_BOUND ( 'NONE', #3573, .T. ) ;
#1820 = EDGE_CURVE ( 'NONE', #11538, #12358, #18096, .T. ) ;
#1821 = DIRECTION ( 'NONE',  ( 0.000000000000000000, 0.000000000000000000, 1.000000000000000000 ) ) ;
#1822 = ORIENTED_EDGE ( 'NONE', *, *, #10528, .T. ) ;
#1823 = EDGE_CURVE ( 'NONE', #7590, #10723, #13722, .T. ) ;
#1824 = LINE ( 'NONE', #11748, #28 ) ;
#1825 = CARTESIAN_POINT ( 'NONE',  ( -57.08002265617300708, 84.22855780814606419, -15.00000000000001421 ) ) ;
#1826 = CYLINDRICAL_SURFACE ( 'NONE', #4828, 12.49999999999999112 ) ;
#1827 = ORIENTED_EDGE ( 'NONE', *, *, #10358, .T. ) ;
#1828 = VECTOR ( 'NONE', #11972, 1000.000000000000000 ) ;
#1829 = LINE ( 'NONE', #3233, #12097 ) ;
#1830 = EDGE_CURVE ( 'NONE', #16012, #583, #766, .T. ) ;
#1831 = EDGE_CURVE ( 'NONE', #2137, #11848, #17201, .T. ) ;
#1832 = DIRECTION ( 'NONE',  ( 0.000000000000000000, 0.000000000000000000, 1.000000000000000000 ) ) ;
#1833 = AXIS2_PLACEMENT_3D ( 'NONE', #11522, #4305, #10972 ) ;
#1834 = ADVANCED_FACE ( 'NONE', ( #1111 ), #9012, .T. ) ;
#1835 = VECTOR ( 'NONE', #10206, 1000.000000000000000 ) ;
#1836 = ORIENTED_EDGE ( 'NONE', *, *, #15430, .F. ) ;
#1837 = ORIENTED_EDGE ( 'NONE', *, *, #14416, .T. ) ;
#1838 = EDGE_CURVE ( 'NONE', #14417, #5330, #4515, .T. ) ;
#1839 = VERTEX_POINT ( 'NONE', #1899 ) ;
#1840 = DIRECTION ( 'NONE',  ( 0.000000000000000000, 0.000000000000000000, 1.000000000000000000 ) ) ;
#1841 = ADVANCED_FACE ( 'NONE', ( #4611 ), #16906, .F. ) ;
#1842 = AXIS2_PLACEMENT_3D ( 'NONE', #6115, #798, #17622 ) ;
#1843 = CARTESIAN_POINT ( 'NONE',  ( -113.4303763223943520, 57.88796029049333214, 26.35917033480641791 ) ) ;
#1844 = CARTESIAN_POINT ( 'NONE',  ( -69.26024277767963611, 81.41924511788803898, -167.1454815528550739 ) ) ;
#1845 = DIRECTION ( 'NONE',  ( -1.000000000000000000, -3.016910393003142859E-15, 0.000000000000000000 ) ) ;
#1846 = DIRECTION ( 'NONE',  ( 0.000000000000000000, 1.000000000000000000, 0.000000000000000000 ) ) ;
#1847 = ORIENTED_EDGE ( 'NONE', *, *, #4139, .T. ) ;
#1848 = LINE ( 'NONE', #448, #5404 ) ;
#1849 = AXIS2_PLACEMENT_3D ( 'NONE', #2031, #2124, #12150 ) ;
#1850 = AXIS2_PLACEMENT_3D ( 'NONE', #5958, #8695, #14315 ) ;
#1851 = CARTESIAN_POINT ( 'NONE',  ( -71.24615306438094819, 66.54966845456371516, -15.00000000000001421 ) ) ;
#1852 = EDGE_CURVE ( 'NONE', #7351, #2768, #9801, .T. ) ;
#1853 = DIRECTION ( 'NONE',  ( -0.000000000000000000, -0.000000000000000000, -1.000000000000000000 ) ) ;
#1854 = CARTESIAN_POINT ( 'NONE',  ( -71.24615306438070661, 135.6647067545637242, -167.1454815528550739 ) ) ;
#1855 = ADVANCED_FACE ( 'NONE', ( #17513 ), #8919, .T. ) ;
#1856 = CARTESIAN_POINT ( 'NONE',  ( -46.65463807863145007, 87.07303407725225952, 15.00000000000009592 ) ) ;
#1857 = DIRECTION ( 'NONE',  ( 0.000000000000000000, -1.000000000000000000, -2.775557561562874095E-16 ) ) ;
#1858 = ORIENTED_EDGE ( 'NONE', *, *, #457, .T. ) ;
#1859 = ADVANCED_FACE ( 'NONE', ( #1633 ), #13321, .T. ) ;
#1860 = AXIS2_PLACEMENT_3D ( 'NONE', #14608, #16017, #12864 ) ;
#1861 = CARTESIAN_POINT ( 'NONE',  ( -56.26901274438541378, 73.45256821284058901, -167.1454815528550739 ) ) ;
#1862 = CARTESIAN_POINT ( 'NONE',  ( -36.12589806422543148, 82.27553650601718971, 55.25452123045118213 ) ) ;
#1863 = ORIENTED_EDGE ( 'NONE', *, *, #4574, .F. ) ;
#1864 = ORIENTED_EDGE ( 'NONE', *, *, #15087, .T. ) ;
#1865 = CIRCLE ( 'NONE', #16187, 10.24900000000000055 ) ;
#1866 = AXIS2_PLACEMENT_3D ( 'NONE', #9872, #6873, #18396 ) ;
#1867 = VERTEX_POINT ( 'NONE', #15936 ) ;
#1868 = CARTESIAN_POINT ( 'NONE',  ( -68.99615306438072082, 127.6737176881302958, -15.00000000000001421 ) ) ;
#1869 = CARTESIAN_POINT ( 'NONE',  ( -68.99615306438111872, 11.43478963813029914, -15.00000000000001421 ) ) ;
#1870 = LINE ( 'NONE', #7578, #15513 ) ;
#1871 = CARTESIAN_POINT ( 'NONE',  ( -68.99615306438117557, 4.536748481662661092, 15.00000000000006928 ) ) ;
#1872 = CIRCLE ( 'NONE', #13239, 9.197489084949710403 ) ;
#1873 = DIRECTION ( 'NONE',  ( 0.000000000000000000, 0.000000000000000000, 1.000000000000000000 ) ) ;
#1874 = CARTESIAN_POINT ( 'NONE',  ( 5.699999999999996625, 0.000000000000000000, 0.000000000000000000 ) ) ;
#1875 = DIRECTION ( 'NONE',  ( 0.000000000000000000, 0.000000000000000000, -1.000000000000000000 ) ) ;
#1876 = EDGE_LOOP ( 'NONE', ( #12983, #14667, #10558, #5358 ) ) ;
#1877 = PLANE ( 'NONE',  #17077 ) ;
#1878 = CARTESIAN_POINT ( 'NONE',  ( -68.99615306438086293, 89.35975003166268493, -167.1454815528550739 ) ) ;
#1879 = AXIS2_PLACEMENT_3D ( 'NONE', #18343, #2618, #8418 ) ;
#1880 = CIRCLE ( 'NONE', #12348, 4.600000000000006750 ) ;
#1881 = PLANE ( 'NONE',  #7756 ) ;
#1882 = ORIENTED_EDGE ( 'NONE', *, *, #3103, .T. ) ;
#1883 = DIRECTION ( 'NONE',  ( 0.000000000000000000, 0.000000000000000000, 1.000000000000000000 ) ) ;
#1884 = DIRECTION ( 'NONE',  ( -1.000000000000000000, -0.000000000000000000, -0.000000000000000000 ) ) ;
#1885 = ORIENTED_EDGE ( 'NONE', *, *, #8517, .T. ) ;
#1886 = AXIS2_PLACEMENT_3D ( 'NONE', #16649, #8687, #3844 ) ;
#1887 = EDGE_LOOP ( 'NONE', ( #13670, #1802, #10861, #14344 ) ) ;
#1888 = CONICAL_SURFACE ( 'NONE', #7865, 3.999999999999982681, 1.029744258676651203 ) ;
#1889 = AXIS2_PLACEMENT_3D ( 'NONE', #2431, #2534, #6639 ) ;
#1890 = VECTOR ( 'NONE', #14889, 1000.000000000000000 ) ;
#1891 = DIRECTION ( 'NONE',  ( 0.000000000000000000, 0.000000000000000000, 1.000000000000000000 ) ) ;
#1892 = LINE ( 'NONE', #16184, #10888 ) ;
#1893 = LINE ( 'NONE', #9372, #7837 ) ;
#1894 = ORIENTED_EDGE ( 'NONE', *, *, #10650, .T. ) ;
#1895 = VERTEX_POINT ( 'NONE', #5999 ) ;
#1896 = B_SPLINE_CURVE_WITH_KNOTS ( 'NONE', 3,
 ( #17852, #5031, #10745, #16439, #13657, #16538, #3740, #2321, #13743, #11137, #6820, #12539, #15232, #18237, #8522, #9732, #7107, #17010 ),
 .UNSPECIFIED., .F., .F.,
 ( 4, 2, 2, 2, 2, 2, 2, 2, 4 ),
 ( 0.002699315152504171492, 0.004615533240672466987, 0.005573642284756619505, 0.006531751328840772891, 0.007489860372924925409, 0.008447969417009077928, 0.008927023939051153753, 0.009406078461093231313, 0.01036418750517741419 ),
 .UNSPECIFIED. ) ;
#1897 = LINE ( 'NONE', #7605, #14378 ) ;
#1898 = DIRECTION ( 'NONE',  ( 1.156482317317869999E-16, 0.000000000000000000, 1.000000000000000000 ) ) ;
#1899 = CARTESIAN_POINT ( 'NONE',  ( -71.24615306438120399, 0.5762228045637918239, -15.00000000000001421 ) ) ;
#1900 = CYLINDRICAL_SURFACE ( 'NONE', #17107, 29.36884788726140627 ) ;
#1901 = ORIENTED_EDGE ( 'NONE', *, *, #10256, .T. ) ;
#1902 = LINE ( 'NONE', #1804, #13137 ) ;
#1903 = ORIENTED_EDGE ( 'NONE', *, *, #2637, .T. ) ;
#1904 = FACE_OUTER_BOUND ( 'NONE', #6363, .T. ) ;
#1905 = CIRCLE ( 'NONE', #16530, 85.91469608272775815 ) ;
#1906 = DIRECTION ( 'NONE',  ( 1.000000000000000000, 0.000000000000000000, 0.000000000000000000 ) ) ;
#1908 = VERTEX_POINT ( 'NONE', #9897 ) ;
#1907 = CIRCLE ( 'NONE', #111, 26.04359719766049608 ) ;
#1909 = EDGE_LOOP ( 'NONE', ( #2214, #7127, #13459, #10693 ) ) ;
#1910 = ORIENTED_EDGE ( 'NONE', *, *, #10499, .F. ) ;
#1911 = DIRECTION ( 'NONE',  ( 1.000000000000000000, 0.000000000000000000, 0.000000000000000000 ) ) ;
#1912 = CARTESIAN_POINT ( 'NONE',  ( -63.91856434051376823, 76.59466308582156557, -15.00000000000001421 ) ) ;
#1913 = ORIENTED_EDGE ( 'NONE', *, *, #309, .T. ) ;
#1914 = CIRCLE ( 'NONE', #15049, 12.58237727243326987 ) ;
#1916 = AXIS2_PLACEMENT_3D ( 'NONE', #9758, #16562, #12379 ) ;
#1915 = DIRECTION ( 'NONE',  ( 0.9396926207859084279, 0.3420201433256686574, -1.086737899652989892E-16 ) ) ;
#1917 = LINE ( 'NONE', #2959, #18274 ) ;
#1918 = PLANE ( 'NONE',  #3131 ) ;
#1919 = ORIENTED_EDGE ( 'NONE', *, *, #8256, .T. ) ;
#1920 = EDGE_CURVE ( 'NONE', #12847, #10167, #11827, .T. ) ;
#1921 = CARTESIAN_POINT ( 'NONE',  ( -107.5926225674731853, 106.8071537307723133, -25.00000000000000000 ) ) ;
#1922 = VERTEX_POINT ( 'NONE', #3129 ) ;
#1923 = DIRECTION ( 'NONE',  ( -0.000000000000000000, 0.000000000000000000, -1.000000000000000000 ) ) ;
#1924 = CARTESIAN_POINT ( 'NONE',  ( -68.99615306438080609, 108.2093059316626693, -15.00000000000001421 ) ) ;
#1925 = VERTEX_POINT ( 'NONE', #1300 ) ;
#1926 = AXIS2_PLACEMENT_3D ( 'NONE', #18097, #873, #16490 ) ;
#1927 = CARTESIAN_POINT ( 'NONE',  ( -92.59262256747321373, 117.8748711238780373, 35.00000000000000000 ) ) ;
#1928 = AXIS2_PLACEMENT_3D ( 'NONE', #1659, #15962, #175 ) ;
#1929 = CARTESIAN_POINT ( 'NONE',  ( -71.24615306438111872, 22.56737135456379661, -167.1454815528550739 ) ) ;
#1930 = VECTOR ( 'NONE', #702, 1000.000000000000114 ) ;
#1931 = VERTEX_POINT ( 'NONE', #4098 ) ;
#1932 = AXIS2_PLACEMENT_3D ( 'NONE', #13369, #17851, #546 ) ;
#1933 = EDGE_CURVE ( 'NONE', #9072, #9564, #8852, .T. ) ;
#1934 = ORIENTED_EDGE ( 'NONE', *, *, #17501, .F. ) ;
#1935 = VERTEX_POINT ( 'NONE', #7415 ) ;
#1936 = LINE ( 'NONE', #2295, #12978 ) ;
#1937 = DIRECTION ( 'NONE',  ( 1.000000000000000000, 0.000000000000000000, 0.000000000000000000 ) ) ;
#1938 = DIRECTION ( 'NONE',  ( -0.000000000000000000, 0.000000000000000000, -1.000000000000000000 ) ) ;
#1939 = LINE ( 'NONE', #7646, #420 ) ;
#1940 = EDGE_LOOP ( 'NONE', ( #1, #17282, #9831, #15588, #12337, #9495 ) ) ;
#1941 = VECTOR ( 'NONE', #8824, 1000.000000000000114 ) ;
#1942 = EDGE_CURVE ( 'NONE', #14058, #17058, #10586, .T. ) ;
#1943 = EDGE_CURVE ( 'NONE', #15911, #13807, #6093, .T. ) ;
#1944 = FACE_BOUND ( 'NONE', #9965, .T. ) ;
#1945 = VECTOR ( 'NONE', #18289, 1000.000000000000000 ) ;
#1946 = DIRECTION ( 'NONE',  ( 1.000000000000000000, 0.000000000000000000, 5.077734830647302671E-16 ) ) ;
#1947 = CARTESIAN_POINT ( 'NONE',  ( -70.85175816390371040, -141.5628872026273086, 18.23991632971911514 ) ) ;
#1948 = VECTOR ( 'NONE', #14398, 1000.000000000000000 ) ;
#1949 = LINE ( 'NONE', #13357, #7829 ) ;
#1950 = LINE ( 'NONE', #5879, #11998 ) ;
#1951 = VERTEX_POINT ( 'NONE', #15841 ) ;
#1952 = ADVANCED_FACE ( 'NONE', ( #8401 ), #14112, .T. ) ;
#1953 = DIRECTION ( 'NONE',  ( 1.000000000000000000, 0.000000000000000000, -0.000000000000000000 ) ) ;
#1954 = EDGE_LOOP ( 'NONE', ( #8661, #729, #3298, #2153 ) ) ;
#1955 = EDGE_CURVE ( 'NONE', #13329, #18188, #11727, .T. ) ;
#1956 = CARTESIAN_POINT ( 'NONE',  ( -92.59262256747318531, -1.909541702982995504E-14, 0.000000000000000000 ) ) ;
#1957 = ORIENTED_EDGE ( 'NONE', *, *, #14986, .T. ) ;
#1958 = EDGE_CURVE ( 'NONE', #6487, #4021, #4185, .T. ) ;
#1959 = ORIENTED_EDGE ( 'NONE', *, *, #1153, .F. ) ;
#1960 = VECTOR ( 'NONE', #12148, 1000.000000000000000 ) ;
#1961 = ADVANCED_FACE ( 'NONE', ( #13227 ), #11306, .T. ) ;
#1962 = AXIS2_PLACEMENT_3D ( 'NONE', #4693, #3032, #13131 ) ;
#1963 = EDGE_CURVE ( 'NONE', #1526, #6914, #14518, .T. ) ;
#1964 = ORIENTED_EDGE ( 'NONE', *, *, #5009, .T. ) ;
#1965 = DIRECTION ( 'NONE',  ( 0.000000000000000000, 0.000000000000000000, 1.000000000000000000 ) ) ;
#1966 = DIRECTION ( 'NONE',  ( -1.000000000000000000, 0.000000000000000000, 0.000000000000000000 ) ) ;
#1967 = CARTESIAN_POINT ( 'NONE',  ( -68.99615306438100504, 48.51904558166270220, -167.1454815528550739 ) ) ;
#1968 = EDGE_CURVE ( 'NONE', #7210, #13855, #12283, .T. ) ;
#1969 = EDGE_CURVE ( 'NONE', #3472, #8476, #8196, .T. ) ;
#1970 = DIRECTION ( 'NONE',  ( 1.000000000000000000, 0.000000000000000000, 0.000000000000000000 ) ) ;
#1971 = LINE ( 'NONE', #7670, #2547 ) ;
#1972 = CARTESIAN_POINT ( 'NONE',  ( -65.50906076758114693, 77.46608744949911340, -167.1454815528550739 ) ) ;
#1973 = ORIENTED_EDGE ( 'NONE', *, *, #6042, .F. ) ;
#1974 = CARTESIAN_POINT ( 'NONE',  ( -36.57592446955339227, 45.96055548693809101, -29.96385110796869000 ) ) ;
#1975 = CARTESIAN_POINT ( 'NONE',  ( -75.82624405736112294, 61.62045879897588918, -27.81207011136935847 ) ) ;
#1976 = CARTESIAN_POINT ( 'NONE',  ( -71.24615306438100504, 53.09442711522921599, 15.00000000000006928 ) ) ;
#1977 = ORIENTED_EDGE ( 'NONE', *, *, #5844, .F. ) ;
#1978 = B_SPLINE_CURVE_WITH_KNOTS ( 'NONE', 3,
 ( #4661, #10374, #3254, #14669, #1862, #7570, #13280, #461, #10834, #4010, #15036, #9438, #742, #17932, #9522, #17844, #6619, #11027, #6520, #2229, #3622, #15132, #2314, #16531, #9723, #7941, #8020, #6435, #5117, #15224, #5021, #12343, #16712, #12236, #9616, #2410, #2612, #10940, #13733, #15320, #12533, #13651, #8116, #6724, #13554, #6812 ),
 .UNSPECIFIED., .F., .F.,
 ( 4, 2, 2, 2, 2, 2, 2, 2, 2, 2, 2, 2, 2, 2, 2, 2, 2, 2, 2, 2, 2, 2, 4 ),
 ( 0.000000000000000000, 0.001477780233738735334, 0.002216670350608105061, 0.002955560467477474570, 0.004433340701216251754, 0.005172230818085658995, 0.005911120934955066235, 0.007388901168693925818, 0.008866681402432782799, 0.009605571519302205652, 0.01034446163617162677, 0.01182224186991048982, 0.01330002210364935461, 0.01477780233738821593, 0.01625558257112707725, 0.01699447268799647928, 0.01773336280486588479, 0.01921114303860466457, 0.01995003315547405273, 0.02068892327234343395, 0.02216670350608219292, 0.02290559362295159149, 0.02364448373982099005 ),
 .UNSPECIFIED. ) ;
#1979 = PLANE ( 'NONE',  #5827 ) ;
#1980 = FACE_OUTER_BOUND ( 'NONE', #6155, .T. ) ;
#1981 = EDGE_LOOP ( 'NONE', ( #8847, #9057, #17581, #5148 ) ) ;
#1982 = EDGE_CURVE ( 'NONE', #12444, #4498, #4897, .T. ) ;
#1983 = ORIENTED_EDGE ( 'NONE', *, *, #18140, .T. ) ;
#1984 = LINE ( 'NONE', #9369, #10395 ) ;
#1985 = CYLINDRICAL_SURFACE ( 'NONE', #2205, 10.24900000000000055 ) ;
#1986 = LINE ( 'NONE', #13395, #15924 ) ;
#1987 = ORIENTED_EDGE ( 'NONE', *, *, #12238, .T. ) ;
#1988 = ORIENTED_EDGE ( 'NONE', *, *, #11789, .T. ) ;
#1989 = DIRECTION ( 'NONE',  ( -0.9396926207859171987, 0.3420201433256444545, 0.000000000000000000 ) ) ;
#1990 = CARTESIAN_POINT ( 'NONE',  ( -107.5926225674731711, 65.58224449241410525, -20.00000000000000355 ) ) ;
#1991 = CARTESIAN_POINT ( 'NONE',  ( -76.83309350041878361, 91.48526692943183036, 60.54251226750088222 ) ) ;
#1992 = CARTESIAN_POINT ( 'NONE',  ( -114.1362093120869758, -92.58100082067042536, 7.070573948080970617 ) ) ;
#1993 = ORIENTED_EDGE ( 'NONE', *, *, #3552, .F. ) ;
#1994 = DIRECTION ( 'NONE',  ( -1.000000000000000000, 0.000000000000000000, 0.000000000000000000 ) ) ;
#1995 = EDGE_LOOP ( 'NONE', ( #11913, #4157 ) ) ;
#1996 = CYLINDRICAL_SURFACE ( 'NONE', #10404, 3.999999999999989786 ) ;
#1997 = ORIENTED_EDGE ( 'NONE', *, *, #18461, .F. ) ;
#1998 = ORIENTED_EDGE ( 'NONE', *, *, #12791, .F. ) ;
#1999 = ORIENTED_EDGE ( 'NONE', *, *, #7664, .F. ) ;
#2000 = LINE ( 'NONE', #10791, #16263 ) ;
#2001 = LINE ( 'NONE', #12297, #12639 ) ;
#2002 = ORIENTED_EDGE ( 'NONE', *, *, #3001, .F. ) ;
#2003 = CARTESIAN_POINT ( 'NONE',  ( -107.5926225674731853, 110.5691553257988460, -26.35917033480641436 ) ) ;
#2004 = CARTESIAN_POINT ( 'NONE',  ( -107.5926225674731711, 57.88796029049330372, -26.35917033480641436 ) ) ;
#2005 = ORIENTED_EDGE ( 'NONE', *, *, #9619, .F. ) ;
#2006 = FACE_OUTER_BOUND ( 'NONE', #3138, .T. ) ;
#2007 = ORIENTED_EDGE ( 'NONE', *, *, #8577, .T. ) ;
#2008 = DIRECTION ( 'NONE',  ( -1.000000000000000000, 0.000000000000000000, 0.000000000000000000 ) ) ;
#2009 = CARTESIAN_POINT ( 'NONE',  ( -0.000000000000000000, -111.0842361345572158, -5.654315315325675328 ) ) ;
#2011 = VERTEX_POINT ( 'NONE', #13402 ) ;
#2010 = EDGE_CURVE ( 'NONE', #8653, #11390, #6438, .T. ) ;
#2012 = CARTESIAN_POINT ( 'NONE',  ( 97.91997734382704266, 84.22855780814606419, 70.00000000000001421 ) ) ;
#2013 = CARTESIAN_POINT ( 'NONE',  ( -80.32997185471215573, -91.18731257919071709, -40.31990080433450885 ) ) ;
#2014 = ORIENTED_EDGE ( 'NONE', *, *, #2838, .F. ) ;
#2015 = ORIENTED_EDGE ( 'NONE', *, *, #7574, .T. ) ;
#2016 = DIRECTION ( 'NONE',  ( 0.000000000000000000, 0.000000000000000000, 1.000000000000000000 ) ) ;
#2017 = FACE_OUTER_BOUND ( 'NONE', #11619, .T. ) ;
#2018 = VERTEX_POINT ( 'NONE', #15078 ) ;
#2019 = PRODUCT_CONTEXT ( 'NONE', #3944, 'mechanical' ) ;
#2020 = FACE_OUTER_BOUND ( 'NONE', #5279, .T. ) ;
#2021 =( LENGTH_UNIT ( ) NAMED_UNIT ( * ) SI_UNIT ( .MILLI., .METRE. ) );
#2022 = APPLICATION_CONTEXT ( 'automotive_design' ) ;
#2023 = LINE ( 'NONE', #14834, #4275 ) ;
#2024 = LINE ( 'NONE', #10364, #11191 ) ;
#2025 = VERTEX_POINT ( 'NONE', #17694 ) ;
#2026 = CARTESIAN_POINT ( 'NONE',  ( -47.88253357122329845, 84.22855780814606419, 92.50000000000000000 ) ) ;
#2027 = CARTESIAN_POINT ( 'NONE',  ( -68.99615306438094819, 51.66063823166267355, -167.1454815528550739 ) ) ;
#2028 = DIRECTION ( 'NONE',  ( -0.7071067811865474617, 0.000000000000000000, 0.7071067811865474617 ) ) ;
#2029 = CARTESIAN_POINT ( 'NONE',  ( 276.3098885457529832, -32.62665103886256190, 7.000000000000010658 ) ) ;
#2030 = AXIS2_PLACEMENT_3D ( 'NONE', #4978, #3296, #784 ) ;
#2031 = CARTESIAN_POINT ( 'NONE',  ( -57.08002265617300708, 84.22855780814606419, 2.999999999999999112 ) ) ;
#2032 = EDGE_LOOP ( 'NONE', ( #5746, #13506, #14740, #11251, #18492, #14246 ) ) ;
#2033 = ADVANCED_FACE ( 'NONE', ( #13776 ), #2081, .T. ) ;
#2034 = DIRECTION ( 'NONE',  ( 0.000000000000000000, 0.000000000000000000, 1.000000000000000000 ) ) ;
#2035 = DIRECTION ( 'NONE',  ( 0.000000000000000000, 0.000000000000000000, 1.000000000000000000 ) ) ;
#2036 = ORIENTED_EDGE ( 'NONE', *, *, #10317, .F. ) ;
#2037 = CARTESIAN_POINT ( 'NONE',  ( -68.99615306438067819, 145.9084177316626949, -15.00000000000001421 ) ) ;
#2038 = LINE ( 'NONE', #272, #304 ) ;
#2039 = ORIENTED_EDGE ( 'NONE', *, *, #17075, .T. ) ;
#2040 = VERTEX_POINT ( 'NONE', #16297 ) ;
#2041 = EDGE_CURVE ( 'NONE', #7016, #17935, #10603, .T. ) ;
#2042 = DIRECTION ( 'NONE',  ( 1.000000000000000000, 0.000000000000000000, 0.000000000000000000 ) ) ;
#2043 = ORIENTED_EDGE ( 'NONE', *, *, #13295, .T. ) ;
#2044 = LINE ( 'NONE', #6337, #7611 ) ;
#2045 = DIRECTION ( 'NONE',  ( 1.000000000000000000, 2.062304371594500494E-16, -2.775557561562890858E-16 ) ) ;
#2046 = CARTESIAN_POINT ( 'NONE',  ( -52.35105328106566702, 95.79950628479642205, -167.1454815528550739 ) ) ;
#2047 = DIRECTION ( 'NONE',  ( 1.000000000000000000, 0.000000000000000000, 0.000000000000000000 ) ) ;
#2048 = EDGE_CURVE ( 'NONE', #833, #4354, #17752, .T. ) ;
#2049 = DIRECTION ( 'NONE',  ( 1.000000000000000000, 0.000000000000000000, 5.551115123125784674E-16 ) ) ;
#2050 = DIRECTION ( 'NONE',  ( 0.000000000000000000, 0.000000000000000000, 1.000000000000000000 ) ) ;
#2051 = PRODUCT ( 'Gear Rack', 'Gear Rack', '', ( #9143 ) ) ;
#2052 = VERTEX_POINT ( 'NONE', #3668 ) ;
#2053 = EDGE_CURVE ( 'NONE', #3000, #12847, #1593, .T. ) ;
#2054 = EDGE_CURVE ( 'NONE', #2374, #15750, #9108, .T. ) ;
#2055 = CARTESIAN_POINT ( 'NONE',  ( -71.24615306438076345, 123.0983361545637109, -15.00000000000001421 ) ) ;
#2056 = CARTESIAN_POINT ( 'NONE',  ( -76.14069299065937457, 61.88532069570636907, -26.17446772214336548 ) ) ;
#2057 = DIRECTION ( 'NONE',  ( 0.3420201433256686574, 0.9396926207859084279, -0.000000000000000000 ) ) ;
#2058 = VECTOR ( 'NONE', #2684, 1000.000000000000000 ) ;
#2059 = VERTEX_POINT ( 'NONE', #5162 ) ;
#2060 = FACE_OUTER_BOUND ( 'NONE', #8644, .T. ) ;
#2061 = DIRECTION ( 'NONE',  ( 0.000000000000000000, 1.000000000000000000, -0.000000000000000000 ) ) ;
#2062 = EDGE_LOOP ( 'NONE', ( #14474, #14620, #14701, #12280, #10684 ) ) ;
#2063 = ADVANCED_FACE ( 'NONE', ( #6369 ), #7694, .F. ) ;
#2064 = EDGE_CURVE ( 'NONE', #14012, #2549, #12075, .T. ) ;
#2065 = ADVANCED_FACE ( 'NONE', ( #3852 ), #1151, .F. ) ;
#2066 = ORIENTED_EDGE ( 'NONE', *, *, #5268, .T. ) ;
#2067 = EDGE_CURVE ( 'NONE', #17780, #8569, #9558, .T. ) ;
#2068 = CARTESIAN_POINT ( 'NONE',  ( -57.08002265617300708, 84.22855780814606419, 37.50000000000000000 ) ) ;
#2069 = DIRECTION ( 'NONE',  ( 1.000000000000000000, 2.062304371594500740E-16, 0.000000000000000000 ) ) ;
#2070 = AXIS2_PLACEMENT_3D ( 'NONE', #14552, #10073, #15773 ) ;
#2071 = FACE_OUTER_BOUND ( 'NONE', #8201, .T. ) ;
#2072 = FACE_OUTER_BOUND ( 'NONE', #7816, .T. ) ;
#2073 = EDGE_CURVE ( 'NONE', #14401, #7613, #15264, .T. ) ;
#2074 = ORIENTED_EDGE ( 'NONE', *, *, #12359, .T. ) ;
#2075 = PLANE ( 'NONE',  #3272 ) ;
#2076 = VECTOR ( 'NONE', #613, 1000.000000000000000 ) ;
#2077 = CARTESIAN_POINT ( 'NONE',  ( -68.99615306438109030, 17.10311908166270456, -167.1454815528550739 ) ) ;
#2078 = VERTEX_POINT ( 'NONE', #3533 ) ;
#2079 = DIRECTION ( 'NONE',  ( 0.3420201433256444545, 0.9396926207859171987, -0.000000000000000000 ) ) ;
#2080 = CARTESIAN_POINT ( 'NONE',  ( -66.30216873316086890, 111.8377431448113555, 25.00000000000000355 ) ) ;
#2081 = PLANE ( 'NONE',  #7307 ) ;
#2082 = DIRECTION ( 'NONE',  ( 0.000000000000000000, 1.000000000000000000, 0.000000000000000000 ) ) ;
#2083 = ORIENTED_EDGE ( 'NONE', *, *, #3300, .T. ) ;
#2084 = EDGE_CURVE ( 'NONE', #14275, #961, #7845, .T. ) ;
#2085 = ADVANCED_FACE ( 'NONE', ( #6335 ), #12064, .T. ) ;
#2086 = DIRECTION ( 'NONE',  ( -0.9396926207859084279, 0.3420201433256686574, 1.086737899652989892E-16 ) ) ;
#2087 = VERTEX_POINT ( 'NONE', #2415 ) ;
#2088 = PLANE ( 'NONE',  #6821 ) ;
#2089 = VERTEX_POINT ( 'NONE', #10740 ) ;
#2090 = VECTOR ( 'NONE', #6349, 1000.000000000000000 ) ;
#2091 = AXIS2_PLACEMENT_3D ( 'NONE', #15772, #2957, #12888 ) ;
#2092 = ORIENTED_EDGE ( 'NONE', *, *, #4008, .T. ) ;
#2093 =( NAMED_UNIT ( * ) SI_UNIT ( $, .STERADIAN. ) SOLID_ANGLE_UNIT ( ) );
#2094 = LINE ( 'NONE', #4984, #4533 ) ;
#2095 = ORIENTED_EDGE ( 'NONE', *, *, #4863, .T. ) ;
#2096 = DIRECTION ( 'NONE',  ( 0.000000000000000000, 0.000000000000000000, 1.000000000000000000 ) ) ;
#2097 = VECTOR ( 'NONE', #3251, 1000.000000000000000 ) ;
#2098 = FACE_OUTER_BOUND ( 'NONE', #1017, .T. ) ;
#2099 = ORIENTED_EDGE ( 'NONE', *, *, #4636, .F. ) ;
#2100 = CARTESIAN_POINT ( 'NONE',  ( -60.06546592763139358, -96.08423613455721579, 28.18308811886542742 ) ) ;
#2101 = AXIS2_PLACEMENT_3D ( 'NONE', #9531, #7851, #3826 ) ;
#2102 = VERTEX_POINT ( 'NONE', #13558 ) ;
#2103 = DIRECTION ( 'NONE',  ( 0.000000000000000000, 0.000000000000000000, 1.000000000000000000 ) ) ;
#2104 = CARTESIAN_POINT ( 'NONE',  ( -57.08002265617300708, 84.22855780814606419, -15.00000000000001421 ) ) ;
#2105 = ORIENTED_EDGE ( 'NONE', *, *, #7355, .T. ) ;
#2106 = DIRECTION ( 'NONE',  ( 0.000000000000000000, 0.000000000000000000, 1.000000000000000000 ) ) ;
#2107 = AXIS2_PLACEMENT_3D ( 'NONE', #11691, #17379, #16342 ) ;
#2108 = DIRECTION ( 'NONE',  ( 0.000000000000000000, -1.000000000000000000, 3.330669073875448914E-16 ) ) ;
#2109 = ORIENTED_EDGE ( 'NONE', *, *, #14412, .F. ) ;
#2110 = CIRCLE ( 'NONE', #615, 85.91469608272775815 ) ;
#2111 = VECTOR ( 'NONE', #3517, 1000.000000000000000 ) ;
#2113 = ADVANCED_FACE ( 'NONE', ( #2233 ), #16628, .T. ) ;
#2112 = DIRECTION ( 'NONE',  ( -1.000000000000000000, 3.114344029463675185E-14, 1.692578276882432005E-16 ) ) ;
#2114 = DIRECTION ( 'NONE',  ( -5.204170427930409450E-16, 0.000000000000000000, 1.000000000000000000 ) ) ;
#2115 = ORIENTED_EDGE ( 'NONE', *, *, #8256, .F. ) ;
#2116 = DIRECTION ( 'NONE',  ( 0.000000000000000000, 0.000000000000000000, -1.000000000000000000 ) ) ;
#2117 = LINE ( 'NONE', #10720, #17712 ) ;
#2118 = LINE ( 'NONE', #15207, #8794 ) ;
#2119 = ORIENTED_EDGE ( 'NONE', *, *, #16116, .T. ) ;
#2120 = AXIS2_PLACEMENT_3D ( 'NONE', #3968, #8182, #13901 ) ;
#2121 = CARTESIAN_POINT ( 'NONE',  ( -107.5926225674731711, -2.218887358722170814E-14, 0.000000000000000000 ) ) ;
#2122 = CARTESIAN_POINT ( 'NONE',  ( -68.99615306438089135, 67.98345733813025049, -167.1454815528550739 ) ) ;
#2123 = CARTESIAN_POINT ( 'NONE',  ( -57.08002265617300708, 84.22855780814606419, -167.1454815528550739 ) ) ;
#2124 = DIRECTION ( 'NONE',  ( 0.000000000000000000, -0.000000000000000000, -1.000000000000000000 ) ) ;
#2125 = EDGE_LOOP ( 'NONE', ( #1987, #12915, #5110, #5381 ) ) ;
#2126 = AXIS2_PLACEMENT_3D ( 'NONE', #9968, #4514, #2862 ) ;
#2127 = VECTOR ( 'NONE', #17715, 1000.000000000000000 ) ;
#2128 = LINE ( 'NONE', #636, #11201 ) ;
#2129 = CYLINDRICAL_SURFACE ( 'NONE', #318, 3.999999999999989786 ) ;
#2130 = VERTEX_POINT ( 'NONE', #9249 ) ;
#2131 = CARTESIAN_POINT ( 'NONE',  ( -68.30128029835485393, 78.72098330317788850, -167.1454815528550739 ) ) ;
#2132 = FACE_OUTER_BOUND ( 'NONE', #14459, .T. ) ;
#2133 = EDGE_LOOP ( 'NONE', ( #7653, #4068, #17292, #12384 ) ) ;
#2134 = ORIENTED_EDGE ( 'NONE', *, *, #4548, .F. ) ;
#2135 = AXIS2_PLACEMENT_3D ( 'NONE', #962, #18080, #1149 ) ;
#2136 = DIRECTION ( 'NONE',  ( -0.004825104377941397994, -0.9999883591161159435, 5.580147892302267848E-19 ) ) ;
#2137 = VERTEX_POINT ( 'NONE', #10839 ) ;
#2138 = VECTOR ( 'NONE', #3851, 1000.000000000000000 ) ;
#2139 = CARTESIAN_POINT ( 'NONE',  ( 276.3098885457529832, -32.62665103886256190, 3.000000000000000000 ) ) ;
#2140 = CARTESIAN_POINT ( 'NONE',  ( -71.24615306438073503, 129.3815214545637104, -167.1454815528550739 ) ) ;
#2141 = CARTESIAN_POINT ( 'NONE',  ( -68.99615306438070661, 118.2489397381302467, 15.00000000000006928 ) ) ;
#2142 = CARTESIAN_POINT ( 'NONE',  ( -71.24615306438084872, 94.82400230456377699, -15.00000000000001421 ) ) ;
#2143 = DIRECTION ( 'NONE',  ( 1.000000000000000000, 0.000000000000000000, 0.000000000000000000 ) ) ;
#2144 = ORIENTED_EDGE ( 'NONE', *, *, #3, .T. ) ;
#2145 = EDGE_CURVE ( 'NONE', #11655, #5840, #14937, .T. ) ;
#2146 = CARTESIAN_POINT ( 'NONE',  ( -74.71885885752763556, 60.74579698922836712, -23.55577225783097362 ) ) ;
#2147 = LINE ( 'NONE', #6829, #4780 ) ;
#2148 = VERTEX_POINT ( 'NONE', #1026 ) ;
#2149 = VECTOR ( 'NONE', #4447, 1000.000000000000000 ) ;
#2150 = DIRECTION ( 'NONE',  ( -1.000000000000000000, -2.062304371594500494E-16, -0.000000000000000000 ) ) ;
#2151 = VECTOR ( 'NONE', #5320, 1000.000000000000000 ) ;
#2152 = CARTESIAN_POINT ( 'NONE',  ( -71.24615306438073503, 128.4926507152292459, 15.00000000000006928 ) ) ;
#2153 = ORIENTED_EDGE ( 'NONE', *, *, #6537, .F. ) ;
#2154 = ADVANCED_FACE ( 'NONE', ( #9168 ), #13460, .T. ) ;
#2155 = ORIENTED_EDGE ( 'NONE', *, *, #8376, .F. ) ;
#2156 = EDGE_CURVE ( 'NONE', #6914, #1526, #8158, .T. ) ;
#2157 = VECTOR ( 'NONE', #3561, 1000.000000000000000 ) ;
#2158 = CARTESIAN_POINT ( 'NONE',  ( -102.4618227840623774, -111.0842361345572158, 57.00000000000000000 ) ) ;
#2159 = CARTESIAN_POINT ( 'NONE',  ( -71.24615306438086293, 101.1071876045637055, -15.00000000000001421 ) ) ;
#2160 = LINE ( 'NONE', #7686, #15678 ) ;
#2161 = DIRECTION ( 'NONE',  ( -0.000000000000000000, -1.000000000000000000, 0.000000000000000000 ) ) ;
#2162 = ORIENTED_EDGE ( 'NONE', *, *, #7545, .T. ) ;
#2163 = VECTOR ( 'NONE', #3558, 1000.000000000000000 ) ;
#2164 = FACE_OUTER_BOUND ( 'NONE', #1556, .T. ) ;
#2165 = ORIENTED_EDGE ( 'NONE', *, *, #9280, .T. ) ;
#2166 = EDGE_CURVE ( 'NONE', #15084, #12932, #645, .T. ) ;
#2167 = CARTESIAN_POINT ( 'NONE',  ( -68.99615306438100504, 42.85071613813029501, -167.1454815528550739 ) ) ;
#2168 = CARTESIAN_POINT ( 'NONE',  ( -71.24615306438080609, 110.5319655545637403, -167.1454815528550739 ) ) ;
#2169 = CARTESIAN_POINT ( 'NONE',  ( -78.23321842955243710, 73.26749283226919829, 97.49999999999998579 ) ) ;
#2170 = ADVANCED_FACE ( 'NONE', ( #14852 ), #3734, .T. ) ;
#2171 = DIRECTION ( 'NONE',  ( -5.204170427930409450E-16, 0.000000000000000000, 1.000000000000000000 ) ) ;
#2172 = ORIENTED_EDGE ( 'NONE', *, *, #7203, .F. ) ;
#2173 = FACE_OUTER_BOUND ( 'NONE', #18405, .T. ) ;
#2174 = ORIENTED_EDGE ( 'NONE', *, *, #4199, .T. ) ;
#2175 = CIRCLE ( 'NONE', #10243, 12.49999999999999112 ) ;
#2176 = DIRECTION ( 'NONE',  ( -1.000000000000000000, -0.000000000000000000, -0.000000000000000000 ) ) ;
#2177 = VERTEX_POINT ( 'NONE', #12160 ) ;
#2178 = EDGE_CURVE ( 'NONE', #15057, #6937, #11751, .T. ) ;
#2179 = VECTOR ( 'NONE', #649, 1000.000000000000000 ) ;
#2180 = AXIS2_PLACEMENT_3D ( 'NONE', #6764, #8165, #1072 ) ;
#2181 = AXIS2_PLACEMENT_3D ( 'NONE', #6034, #4384, #2976 ) ;
#2182 = EDGE_CURVE ( 'NONE', #10531, #9679, #13248, .T. ) ;
#2183 = ORIENTED_EDGE ( 'NONE', *, *, #2073, .T. ) ;
#2184 = EDGE_CURVE ( 'NONE', #18220, #11731, #18040, .T. ) ;
#2185 = CARTESIAN_POINT ( 'NONE',  ( -70.71978124295668522, -96.08423613455721579, -28.18308811886538479 ) ) ;
#2186 = EDGE_CURVE ( 'NONE', #6852, #11754, #7944, .T. ) ;
#2187 = DIRECTION ( 'NONE',  ( 0.000000000000000000, 0.000000000000000000, 1.000000000000000000 ) ) ;
#2188 = ORIENTED_EDGE ( 'NONE', *, *, #9489, .F. ) ;
#2189 = DIRECTION ( 'NONE',  ( -1.000000000000000000, -0.000000000000000000, -0.000000000000000000 ) ) ;
#2190 = DIRECTION ( 'NONE',  ( 1.000000000000000000, 0.000000000000000000, 3.771137991253928573E-16 ) ) ;
#2191 = VERTEX_POINT ( 'NONE', #5122 ) ;
#2192 = EDGE_CURVE ( 'NONE', #8653, #10149, #14444, .T. ) ;
#2193 = LINE ( 'NONE', #5080, #16443 ) ;
#2194 =( GEOMETRIC_REPRESENTATION_CONTEXT ( 3 ) GLOBAL_UNCERTAINTY_ASSIGNED_CONTEXT ( ( #12468 ) ) GLOBAL_UNIT_ASSIGNED_CONTEXT ( ( #10446, #10543, #16139 ) ) REPRESENTATION_CONTEXT ( 'NONE', 'WORKASPACE' ) );
#2195 = AXIS2_PLACEMENT_3D ( 'NONE', #3510, #5002, #17909 ) ;
#2196 = ORIENTED_EDGE ( 'NONE', *, *, #12976, .T. ) ;
#2197 = VECTOR ( 'NONE', #722, 1000.000000000000114 ) ;
#2198 = CARTESIAN_POINT ( 'NONE',  ( -68.99615306438097662, 61.08541618166268705, 15.00000000000006928 ) ) ;
#2199 = CARTESIAN_POINT ( 'NONE',  ( -66.09703808151903104, 109.8904997453310557, 24.99999999999999645 ) ) ;
#2200 = ORIENTED_EDGE ( 'NONE', *, *, #7616, .F. ) ;
#2201 = DIRECTION ( 'NONE',  ( 0.000000000000000000, 1.000000000000000000, 0.000000000000000000 ) ) ;
#2202 = CARTESIAN_POINT ( 'NONE',  ( -76.42964172313168092, -95.23217669033338950, -44.98760873426162021 ) ) ;
#2203 = ORIENTED_EDGE ( 'NONE', *, *, #8507, .T. ) ;
#2204 = AXIS2_PLACEMENT_3D ( 'NONE', #13352, #8877, #11943 ) ;
#2205 = AXIS2_PLACEMENT_3D ( 'NONE', #13488, #9278, #571 ) ;
#2206 = ORIENTED_EDGE ( 'NONE', *, *, #17842, .T. ) ;
#2207 = LINE ( 'NONE', #7920, #1023 ) ;
#2208 = CARTESIAN_POINT ( 'NONE',  ( -68.99615306438074924, 121.3905323881302962, -167.1454815528550739 ) ) ;
#2209 = ORIENTED_EDGE ( 'NONE', *, *, #15596, .F. ) ;
#2210 = DIRECTION ( 'NONE',  ( 0.000000000000000000, 1.000000000000000000, 0.000000000000000000 ) ) ;
#2211 = CARTESIAN_POINT ( 'NONE',  ( -77.89415131665849401, 81.12099773066752562, 55.66971324650689468 ) ) ;
#2212 = CARTESIAN_POINT ( 'NONE',  ( 3.839371739003430761, -5.119679209322452351, 51.89990490011624047 ) ) ;
#2213 = FACE_OUTER_BOUND ( 'NONE', #9873, .T. ) ;
#2214 = ORIENTED_EDGE ( 'NONE', *, *, #4450, .F. ) ;
#2215 = VECTOR ( 'NONE', #12400, 1000.000000000000000 ) ;
#2216 = PLANE ( 'NONE',  #2717 ) ;
#2217 = LINE ( 'NONE', #16616, #4948 ) ;
#2218 = CARTESIAN_POINT ( 'NONE',  ( -57.08002265617300708, 84.22855780814606419, -167.1454815528550739 ) ) ;
#2219 = CARTESIAN_POINT ( 'NONE',  ( -67.59262256747317110, 57.88796029049329661, 26.35917033480641436 ) ) ;
#2220 = ORIENTED_EDGE ( 'NONE', *, *, #10741, .F. ) ;
#2221 = CIRCLE ( 'NONE', #8525, 9.999999999999994671 ) ;
#2222 = CIRCLE ( 'NONE', #7308, 6.500000000000039968 ) ;
#2223 = CIRCLE ( 'NONE', #7309, 12.50000000000001776 ) ;
#2224 = DIRECTION ( 'NONE',  ( 0.000000000000000000, 0.000000000000000000, 1.000000000000000000 ) ) ;
#2225 = CARTESIAN_POINT ( 'NONE',  ( -57.08002265617300708, 84.22855780814606419, -28.00000000000000355 ) ) ;
#2226 = EDGE_LOOP ( 'NONE', ( #3857, #16310, #14901, #4681 ) ) ;
#2227 = PRODUCT_DEFINITION ( 'UNKNOWN', '', #11173, #6257 ) ;
#2228 = CARTESIAN_POINT ( 'NONE',  ( -68.99615306438111872, 14.57638228813026871, 15.00000000000006928 ) ) ;
#2229 = CARTESIAN_POINT ( 'NONE',  ( -37.32251811057857793, 76.98425793134822470, 60.54272255928178481 ) ) ;
#2230 = ORIENTED_EDGE ( 'NONE', *, *, #704, .F. ) ;
#2231 = VERTEX_POINT ( 'NONE', #15135 ) ;
#2232 = VECTOR ( 'NONE', #13767, 1000.000000000000000 ) ;
#2233 = FACE_OUTER_BOUND ( 'NONE', #6669, .T. ) ;
#2234 = VECTOR ( 'NONE', #4103, 1000.000000000000000 ) ;
#2235 = ORIENTED_EDGE ( 'NONE', *, *, #9721, .T. ) ;
#2236 = AXIS2_PLACEMENT_3D ( 'NONE', #5521, #18049, #2427 ) ;
#2237 = AXIS2_PLACEMENT_3D ( 'NONE', #12474, #11059, #16746 ) ;
#2238 = CARTESIAN_POINT ( 'NONE',  ( -92.59262256747319952, 54.12595869546677818, 25.00000000000000000 ) ) ;
#2239 = CARTESIAN_POINT ( 'NONE',  ( -70.27900850916093134, -47.21335801510345220, -15.00000000000001599 ) ) ;
#2240 = CARTESIAN_POINT ( 'NONE',  ( -66.17391212418095847, 57.96819926477352425, -28.00000000000000000 ) ) ;
#2241 = DIRECTION ( 'NONE',  ( 0.000000000000000000, 1.000000000000000000, 0.000000000000000000 ) ) ;
#2242 = DIRECTION ( 'NONE',  ( 1.000000000000000000, 0.000000000000000000, 3.771137991253934490E-16 ) ) ;
#2243 = FACE_OUTER_BOUND ( 'NONE', #17880, .T. ) ;
#2244 = ORIENTED_EDGE ( 'NONE', *, *, #5261, .F. ) ;
#2245 = DIRECTION ( 'NONE',  ( 0.000000000000000000, 1.000000000000000000, 0.000000000000000000 ) ) ;
#2246 = CARTESIAN_POINT ( 'NONE',  ( -49.40461175531926585, 94.09456345901895702, -167.1454815528550739 ) ) ;
#2247 = VERTEX_POINT ( 'NONE', #6623 ) ;
#2248 = EDGE_CURVE ( 'NONE', #4300, #12168, #2317, .T. ) ;
#2249 = AXIS2_PLACEMENT_3D ( 'NONE', #1277, #9879, #13042 ) ;
#2250 = EDGE_CURVE ( 'NONE', #18326, #9192, #5608, .T. ) ;
#2251 =( GEOMETRIC_REPRESENTATION_CONTEXT ( 3 ) GLOBAL_UNCERTAINTY_ASSIGNED_CONTEXT ( ( #1235 ) ) GLOBAL_UNIT_ASSIGNED_CONTEXT ( ( #17113, #10019, #12920 ) ) REPRESENTATION_CONTEXT ( 'NONE', 'WORKASPACE' ) );
#2252 = FACE_OUTER_BOUND ( 'NONE', #17882, .T. ) ;
#2253 = ORIENTED_EDGE ( 'NONE', *, *, #16029, .F. ) ;
#2254 = ORIENTED_EDGE ( 'NONE', *, *, #3450, .T. ) ;
#2255 = EDGE_CURVE ( 'NONE', #13790, #1045, #16822, .T. ) ;
#2256 = DIRECTION ( 'NONE',  ( -1.000000000000000000, -0.000000000000000000, -0.000000000000000000 ) ) ;
#2257 = DIRECTION ( 'NONE',  ( 0.000000000000000000, 0.000000000000000000, 1.000000000000000000 ) ) ;
#2258 = FACE_OUTER_BOUND ( 'NONE', #4938, .T. ) ;
#2259 = DIRECTION ( 'NONE',  ( -0.000000000000000000, -0.000000000000000000, -1.000000000000000000 ) ) ;
#2260 = CARTESIAN_POINT ( 'NONE',  ( -92.59262256747321373, 114.3311569208253786, 25.00000000000000000 ) ) ;
#2261 = DIRECTION ( 'NONE',  ( 0.000000000000000000, 0.000000000000000000, -1.000000000000000000 ) ) ;
#2262 = ORIENTED_EDGE ( 'NONE', *, *, #6058, .F. ) ;
#2263 = CARTESIAN_POINT ( 'NONE',  ( -71.24615306438106188, 34.24487121522926003, 15.00000000000006928 ) ) ;
#2264 = CARTESIAN_POINT ( 'NONE',  ( -70.27900850916086029, -2.213358015103419341, 15.00000000000006928 ) ) ;
#2265 = CARTESIAN_POINT ( 'NONE',  ( -71.24615306438100504, 53.98329785456373742, -167.1454815528550739 ) ) ;
#2266 = DIRECTION ( 'NONE',  ( 1.000000000000000000, 0.000000000000000000, 3.771137991253934490E-16 ) ) ;
#2267 = ORIENTED_EDGE ( 'NONE', *, *, #3675, .F. ) ;
#2268 = FACE_OUTER_BOUND ( 'NONE', #1954, .T. ) ;
#2269 = ORIENTED_EDGE ( 'NONE', *, *, #17911, .T. ) ;
#2270 = DIRECTION ( 'NONE',  ( 0.000000000000000000, 1.000000000000000000, 0.000000000000000000 ) ) ;
#2271 = VERTEX_POINT ( 'NONE', #16824 ) ;
#2272 = VERTEX_POINT ( 'NONE', #1316 ) ;
#2273 = ADVANCED_FACE ( 'NONE', ( #5594 ), #8518, .T. ) ;
#2274 = LINE ( 'NONE', #15279, #11732 ) ;
#2275 = ORIENTED_EDGE ( 'NONE', *, *, #16092, .F. ) ;
#2276 = DIRECTION ( 'NONE',  ( 0.000000000000000000, 0.000000000000000000, -1.000000000000000000 ) ) ;
#2277 = CARTESIAN_POINT ( 'NONE',  ( -92.59262256747319952, 60.58224449241411946, -35.00000000000000000 ) ) ;
#2278 = VERTEX_POINT ( 'NONE', #9910 ) ;
#2279 = DIRECTION ( 'NONE',  ( -5.204170427930409450E-16, 0.000000000000000000, 1.000000000000000000 ) ) ;
#2280 = CYLINDRICAL_SURFACE ( 'NONE', #15870, 5.000000000000000000 ) ;
#2281 = ADVANCED_FACE ( 'NONE', ( #2705 ), #1121, .T. ) ;
#2282 = ORIENTED_EDGE ( 'NONE', *, *, #11444, .T. ) ;
#2283 = EDGE_CURVE ( 'NONE', #14959, #8437, #16516, .T. ) ;
#2284 = CARTESIAN_POINT ( 'NONE',  ( -71.65892208273831443, 109.7273330359258665, -22.44256693161642247 ) ) ;
#2285 = CARTESIAN_POINT ( 'NONE',  ( 0.5805565836007609004, -3.752776749732685158, 6.500000000000043521 ) ) ;
#2286 = ADVANCED_FACE ( 'NONE', ( #12449 ), #7020, .T. ) ;
#2287 = DIRECTION ( 'NONE',  ( -0.000000000000000000, -0.000000000000000000, 1.000000000000000000 ) ) ;
#2288 = ADVANCED_FACE ( 'NONE', ( #6816 ), #1403, .T. ) ;
#2289 = CARTESIAN_POINT ( 'NONE',  ( -78.76908973550854398, -91.80660034481559251, -42.25011218277860081 ) ) ;
#2290 = ORIENTED_EDGE ( 'NONE', *, *, #13858, .T. ) ;
#2291 = EDGE_CURVE ( 'NONE', #9785, #11807, #12812, .T. ) ;
#2292 = ADVANCED_FACE ( 'NONE', ( #10008 ), #15431, .F. ) ;
#2293 = EDGE_CURVE ( 'NONE', #15245, #16207, #12739, .T. ) ;
#2294 = ORIENTED_EDGE ( 'NONE', *, *, #13854, .T. ) ;
#2295 = CARTESIAN_POINT ( 'NONE',  ( -64.22944241949029731, 91.57211267264378307, -167.1454815528550739 ) ) ;
#2296 = CARTESIAN_POINT ( 'NONE',  ( -50.99714023269321217, 75.97988867778809663, -167.1454815528550739 ) ) ;
#2297 = VERTEX_POINT ( 'NONE', #5408 ) ;
#2298 = EDGE_CURVE ( 'NONE', #17894, #16077, #2615, .T. ) ;
#2299 = CARTESIAN_POINT ( 'NONE',  ( -77.74594894602464024, 80.25424057604627137, 56.13491590375404172 ) ) ;
#2300 = CARTESIAN_POINT ( 'NONE',  ( 9.543663295069050534, 56.41207303426870112, 7.000000000000010658 ) ) ;
#2301 = DIRECTION ( 'NONE',  ( 0.000000000000000000, 0.000000000000000000, 1.000000000000000000 ) ) ;
#2302 = ORIENTED_EDGE ( 'NONE', *, *, #14625, .T. ) ;
#2303 = CARTESIAN_POINT ( 'NONE',  ( 105.4583593777968105, 56.41207303426870112, 7.000000000000010658 ) ) ;
#2304 = DIRECTION ( 'NONE',  ( 1.000000000000000000, 0.000000000000000000, 0.000000000000000000 ) ) ;
#2305 = FACE_OUTER_BOUND ( 'NONE', #253, .T. ) ;
#2306 = CARTESIAN_POINT ( 'NONE',  ( -23.67723694629486531, 50.34933454821165810, 27.07273111978159008 ) ) ;
#2307 = VERTEX_POINT ( 'NONE', #18340 ) ;
#2308 = ADVANCED_FACE ( 'NONE', ( #5510, #11234 ), #16920, .F. ) ;
#2309 = DIRECTION ( 'NONE',  ( 0.000000000000000000, 1.000000000000000000, 0.000000000000000000 ) ) ;
#2310 = CARTESIAN_POINT ( 'NONE',  ( -97.59262256747318531, 50.58224449241411236, 25.00000000000000000 ) ) ;
#2311 = EDGE_CURVE ( 'NONE', #845, #113, #18431, .T. ) ;
#2312 = ORIENTED_EDGE ( 'NONE', *, *, #2311, .F. ) ;
#2313 = DIRECTION ( 'NONE',  ( 0.3420201433256481738, 0.9396926207859158664, -0.000000000000000000 ) ) ;
#2314 = CARTESIAN_POINT ( 'NONE',  ( -37.41820911104731806, 76.72881973191589111, 62.00219528655608059 ) ) ;
#2315 = VERTEX_POINT ( 'NONE', #4459 ) ;
#2316 = ORIENTED_EDGE ( 'NONE', *, *, #17517, .F. ) ;
#2317 = LINE ( 'NONE', #8024, #6348 ) ;
#2318 = ADVANCED_BREP_SHAPE_REPRESENTATION ( '', ( #12580, #16217 ), #9669 ) ;
#2319 = ORIENTED_EDGE ( 'NONE', *, *, #2908, .T. ) ;
#2320 = CARTESIAN_POINT ( 'NONE',  ( -57.08002265617300708, 84.22855780814606419, -15.00000000000000711 ) ) ;
#2321 = CARTESIAN_POINT ( 'NONE',  ( -73.62877340657378511, 59.96410525291461369, 22.93460344427330000 ) ) ;
#2322 = DIRECTION ( 'NONE',  ( 0.000000000000000000, 0.000000000000000000, 1.000000000000000000 ) ) ;
#2323 = LINE ( 'NONE', #15048, #6891 ) ;
#2324 = DIRECTION ( 'NONE',  ( 0.000000000000000000, 1.000000000000000000, 0.000000000000000000 ) ) ;
#2325 = CARTESIAN_POINT ( 'NONE',  ( -92.59262256747321373, 107.8748711238780373, -25.00000000000000000 ) ) ;
#2326 = DIRECTION ( 'NONE',  ( -1.000000000000000000, 0.000000000000000000, -0.000000000000000000 ) ) ;
#2327 = VERTEX_POINT ( 'NONE', #16137 ) ;
#2328 = DIRECTION ( 'NONE',  ( -0.000000000000000000, 1.000000000000000000, 0.000000000000000000 ) ) ;
#2329 = CARTESIAN_POINT ( 'NONE',  ( -57.74389692835771370, 95.01461175692088545, 15.00000000000006928 ) ) ;
#2330 = VERTEX_POINT ( 'NONE', #17199 ) ;
#2331 = DIRECTION ( 'NONE',  ( -0.000000000000000000, 0.000000000000000000, -1.000000000000000000 ) ) ;
#2332 = DIRECTION ( 'NONE',  ( 0.000000000000000000, 0.000000000000000000, -1.000000000000000000 ) ) ;
#2333 = ORIENTED_EDGE ( 'NONE', *, *, #16248, .T. ) ;
#2334 = TOROIDAL_SURFACE ( 'NONE', #17864, 40.40389983439752086, 5.000000000000000000 ) ;
#2335 = ORIENTED_EDGE ( 'NONE', *, *, #1160, .T. ) ;
#2336 = EDGE_LOOP ( 'NONE', ( #8107, #15470, #9093, #6408 ) ) ;
#2337 = UNCERTAINTY_MEASURE_WITH_UNIT (LENGTH_MEASURE( 1.000000000000000082E-05 ), #8875, 'distance_accuracy_value', 'NONE');
#2338 = CARTESIAN_POINT ( 'NONE',  ( -71.24615306438087714, 66.54966845456374358, 15.00000000000006928 ) ) ;
#2339 = PLANE ( 'NONE',  #12656 ) ;
#2340 = DIRECTION ( 'NONE',  ( -0.000000000000000000, -0.000000000000000000, -1.000000000000000000 ) ) ;
#2341 = ADVANCED_FACE ( 'NONE', ( #8957 ), #14483, .T. ) ;
#2342 = CARTESIAN_POINT ( 'NONE',  ( -92.59262256747318531, 0.3328663868096687350, -25.00000000000000000 ) ) ;
#2343 = CARTESIAN_POINT ( 'NONE',  ( -40.83486628351231218, 66.64375664990294013, 97.49999999999998579 ) ) ;
#2344 = CARTESIAN_POINT ( 'NONE',  ( -68.99615306438080609, 105.0677132816627051, 15.00000000000006928 ) ) ;
#2345 = ORIENTED_EDGE ( 'NONE', *, *, #14096, .T. ) ;
#2346 = LINE ( 'NONE', #2167, #5422 ) ;
#2347 = DIRECTION ( 'NONE',  ( 0.9396926207859043201, 0.3420201433256802037, 4.890320548438427212E-16 ) ) ;
#2350 = EDGE_CURVE ( 'NONE', #12214, #4736, #2807, .T. ) ;
#2349 = ORIENTED_EDGE ( 'NONE', *, *, #2350, .T. ) ;
#2348 = DIRECTION ( 'NONE',  ( 0.000000000000000000, 1.000000000000000000, 0.000000000000000000 ) ) ;
#2351 = DIRECTION ( 'NONE',  ( 0.000000000000000000, 0.000000000000000000, 1.000000000000000000 ) ) ;
#2352 = DIRECTION ( 'NONE',  ( -1.000000000000000000, 0.000000000000000000, 0.000000000000000000 ) ) ;
#2353 = EDGE_LOOP ( 'NONE', ( #11971, #7688, #1169, #7959 ) ) ;
#2354 = CARTESIAN_POINT ( 'NONE',  ( -68.99615306438094819, 70.51019413166270056, -15.00000000000001421 ) ) ;
#2355 = ORIENTED_EDGE ( 'NONE', *, *, #16481, .F. ) ;
#2356 = PRODUCT_DEFINITION_SHAPE ( 'NONE', 'NONE',  #18526 ) ;
#2357 = EDGE_LOOP ( 'NONE', ( #11397, #13604, #10066, #13559 ) ) ;
#2358 = CIRCLE ( 'NONE', #16701, 4.599999999999999645 ) ;
#2359 = DIRECTION ( 'NONE',  ( -1.000000000000000000, -0.000000000000000000, -0.000000000000000000 ) ) ;
#2360 = CARTESIAN_POINT ( 'NONE',  ( -57.08002265617300708, 84.22855780814606419, 15.00000000000006928 ) ) ;
#2361 = DIRECTION ( 'NONE',  ( 0.000000000000000000, 1.000000000000000000, 0.000000000000000000 ) ) ;
#2362 = VERTEX_POINT ( 'NONE', #8872 ) ;
#2363 = PRODUCT_CONTEXT ( 'NONE', #7518, 'mechanical' ) ;
#2364 = FACE_OUTER_BOUND ( 'NONE', #17216, .T. ) ;
#2365 = DIRECTION ( 'NONE',  ( 1.000000000000000000, 0.000000000000000000, 0.000000000000000000 ) ) ;
#2366 = ORIENTED_EDGE ( 'NONE', *, *, #7655, .T. ) ;
#2367 = DIRECTION ( 'NONE',  ( 4.124608743189000987E-16, -1.000000000000000000, 0.000000000000000000 ) ) ;
#2368 = CARTESIAN_POINT ( 'NONE',  ( -68.99615306438089135, 86.21815738166266385, -167.1454815528550739 ) ) ;
#2369 = DIRECTION ( 'NONE',  ( 0.000000000000000000, 5.551115123125747573E-17, 1.000000000000000000 ) ) ;
#2370 = ORIENTED_EDGE ( 'NONE', *, *, #7643, .T. ) ;
#2371 = CIRCLE ( 'NONE', #5052, 10.24900000000001477 ) ;
#2372 = CARTESIAN_POINT ( 'NONE',  ( -75.30099397498476321, 107.2622484790587407, -24.10072931937693141 ) ) ;
#2373 = DIRECTION ( 'NONE',  ( -0.000000000000000000, -1.000000000000000000, -0.000000000000000000 ) ) ;
#2374 = VERTEX_POINT ( 'NONE', #15791 ) ;
#2375 = EDGE_CURVE ( 'NONE', #15333, #12447, #11163, .T. ) ;
#2376 = VECTOR ( 'NONE', #8342, 1000.000000000000000 ) ;
#2377 = DIRECTION ( 'NONE',  ( 1.000000000000000000, 0.000000000000000000, 0.000000000000000000 ) ) ;
#2378 =( REPRESENTATION_RELATIONSHIP ('NONE','NONE', #359, #15553 ) REPRESENTATION_RELATIONSHIP_WITH_TRANSFORMATION ( #35 )SHAPE_REPRESENTATION_RELATIONSHIP( ) );
#2379 = DIRECTION ( 'NONE',  ( 0.000000000000000000, 1.000000000000000000, -0.000000000000000000 ) ) ;
#2380 = ORIENTED_EDGE ( 'NONE', *, *, #10405, .T. ) ;
#2382 = ADVANCED_FACE ( 'NONE', ( #9050 ), #7373, .T. ) ;
#2381 = CIRCLE ( 'NONE', #12873, 17.12963335357822814 ) ;
#2383 = CARTESIAN_POINT ( 'NONE',  ( -57.08002265617300708, 84.22855780814606419, 15.00000000000006928 ) ) ;
#2384 = DIRECTION ( 'NONE',  ( -0.9396926207859158664, 0.3420201433256481738, 0.000000000000000000 ) ) ;
#2385 = EDGE_CURVE ( 'NONE', #11275, #197, #10171, .T. ) ;
#2386 = ORIENTED_EDGE ( 'NONE', *, *, #2186, .F. ) ;
#2387 = AXIS2_PLACEMENT_3D ( 'NONE', #12250, #17944, #5129 ) ;
#2388 = CARTESIAN_POINT ( 'NONE',  ( -71.24615306438079188, 88.54081700456376325, 15.00000000000006928 ) ) ;
#2389 = CARTESIAN_POINT ( 'NONE',  ( -77.09623126797262671, 77.72742355542474968, 58.72881290435446289 ) ) ;
#2390 = AXIS2_PLACEMENT_3D ( 'NONE', #6723, #5310, #916 ) ;
#2391 = DIRECTION ( 'NONE',  ( -0.000000000000000000, -0.000000000000000000, -1.000000000000000000 ) ) ;
#2392 = CARTESIAN_POINT ( 'NONE',  ( -47.02742034342072941, 91.65790412808885890, -15.00000000000001421 ) ) ;
#2393 = ORIENTED_EDGE ( 'NONE', *, *, #14584, .T. ) ;
#2394 = CARTESIAN_POINT ( 'NONE',  ( -68.99615306438094819, 70.51019413166270056, 15.00000000000006928 ) ) ;
#2395 = CARTESIAN_POINT ( 'NONE',  ( -67.88623620617454435, 84.15481808402788033, -167.1454815528550739 ) ) ;
#2396 = DIRECTION ( 'NONE',  ( 1.000000000000000000, 0.000000000000000000, 0.000000000000000000 ) ) ;
#2397 = FACE_OUTER_BOUND ( 'NONE', #4607, .T. ) ;
#2398 = DIRECTION ( 'NONE',  ( 0.000000000000000000, 0.000000000000000000, -1.000000000000000000 ) ) ;
#2399 = ORIENTED_EDGE ( 'NONE', *, *, #4688, .F. ) ;
#2400 = ADVANCED_FACE ( 'NONE', ( #1663 ), #16049, .T. ) ;
#2401 = AXIS2_PLACEMENT_3D ( 'NONE', #8513, #9810, #2699 ) ;
#2402 = ADVANCED_FACE ( 'NONE', ( #80 ), #4547, .T. ) ;
#2403 = EDGE_CURVE ( 'NONE', #5840, #5095, #13540, .T. ) ;
#2404 = CARTESIAN_POINT ( 'NONE',  ( -68.99615306438106188, 23.38630438166270054, -15.00000000000001421 ) ) ;
#2405 = CARTESIAN_POINT ( 'NONE',  ( -62.15805688404169160, -91.53392936304808813, 41.62626455281458249 ) ) ;
#2406 = VECTOR ( 'NONE', #1225, 1000.000000000000114 ) ;
#2407 = VERTEX_POINT ( 'NONE', #11763 ) ;
#2408 = CARTESIAN_POINT ( 'NONE',  ( -57.08002265617300708, 84.22855780814606419, 68.73600986863397111 ) ) ;
#2409 = VECTOR ( 'NONE', #3151, 1000.000000000000000 ) ;
#2410 = CARTESIAN_POINT ( 'NONE',  ( -36.41409636632135971, 80.25424057604624295, 68.86508409624599381 ) ) ;
#2411 = ORIENTED_EDGE ( 'NONE', *, *, #11467, .F. ) ;
#2412 = AXIS2_PLACEMENT_3D ( 'NONE', #1476, #15613, #2894 ) ;
#2413 = ORIENTED_EDGE ( 'NONE', *, *, #1475, .F. ) ;
#2414 = EDGE_CURVE ( 'NONE', #10920, #17012, #10253, .T. ) ;
#2415 = CARTESIAN_POINT ( 'NONE',  ( -92.59262256747321373, 110.5691553257988460, -30.35917033480641081 ) ) ;
#2416 = PRESENTATION_LAYER_ASSIGNMENT (  '', '', ( #8709 ) ) ;
#2417 = ORIENTED_EDGE ( 'NONE', *, *, #3676, .T. ) ;
#2418 = EDGE_CURVE ( 'NONE', #10909, #17887, #10092, .T. ) ;
#2419 = CARTESIAN_POINT ( 'NONE',  ( -68.99615306438101925, 17.71797493813025781, 15.00000000000006928 ) ) ;
#2420 = DIRECTION ( 'NONE',  ( -0.9396926207859084279, 0.3420201433256686574, -4.890320548438448905E-16 ) ) ;
#2421 = EDGE_CURVE ( 'NONE', #17891, #4300, #13836, .T. ) ;
#2422 = CARTESIAN_POINT ( 'NONE',  ( -68.99615306438086293, 93.11619853813030545, -15.00000000000001421 ) ) ;
#2423 = LINE ( 'NONE', #932, #15542 ) ;
#2424 = AXIS2_PLACEMENT_3D ( 'NONE', #4444, #10157, #11493 ) ;
#2425 = AXIS2_PLACEMENT_3D ( 'NONE', #16211, #16392, #9481 ) ;
#2426 = LINE ( 'NONE', #13660, #11813 ) ;
#2427 = DIRECTION ( 'NONE',  ( 1.000000000000000000, 0.000000000000000000, 0.000000000000000000 ) ) ;
#2428 = LINE ( 'NONE', #5131, #4251 ) ;
#2429 = ORIENTED_EDGE ( 'NONE', *, *, #9390, .T. ) ;
#2430 = EDGE_CURVE ( 'NONE', #16406, #17849, #17359, .T. ) ;
#2431 = CARTESIAN_POINT ( 'NONE',  ( -62.11705611183893438, 93.78931001713317528, -15.00000000000001421 ) ) ;
#2432 = LINE ( 'NONE', #15244, #1527 ) ;
#2433 = VERTEX_POINT ( 'NONE', #6125 ) ;
#2434 = VECTOR ( 'NONE', #5211, 1000.000000000000000 ) ;
#2435 = CARTESIAN_POINT ( 'NONE',  ( -29.41692657362415275, -91.42293623445492301, -8.824457138344822482 ) ) ;
#2436 = LINE ( 'NONE', #3646, #14886 ) ;
#2437 = EDGE_LOOP ( 'NONE', ( #11266, #13234, #13523, #9074 ) ) ;
#2438 = ORIENTED_EDGE ( 'NONE', *, *, #6742, .T. ) ;
#2439 = AXIS2_PLACEMENT_3D ( 'NONE', #17290, #454, #8698 ) ;
#2440 = AXIS2_PLACEMENT_3D ( 'NONE', #5540, #18168, #13966 ) ;
#2441 = ORIENTED_EDGE ( 'NONE', *, *, #17055, .T. ) ;
#2442 = CARTESIAN_POINT ( 'NONE',  ( -123.4618227840623632, -151.5628872026273086, -57.00000000000000000 ) ) ;
#2443 = DIRECTION ( 'NONE',  ( 0.000000000000000000, 1.000000000000000000, 0.000000000000000000 ) ) ;
#2444 = DIRECTION ( 'NONE',  ( 0.000000000000000000, 0.000000000000000000, -1.000000000000000000 ) ) ;
#2445 = CARTESIAN_POINT ( 'NONE',  ( -36.44155368744861079, 56.74635804676025685, 0.000000000000000000 ) ) ;
#2446 = VECTOR ( 'NONE', #1011, 1000.000000000000000 ) ;
#2447 = DIRECTION ( 'NONE',  ( -4.675871521838984962E-16, 1.000000000000000000, 0.000000000000000000 ) ) ;
#2448 = PLANE ( 'NONE',  #2237 ) ;
#2449 = CARTESIAN_POINT ( 'NONE',  ( -49.58002265617300708, 84.22855780814606419, -15.00000000000001421 ) ) ;
#2450 = VERTEX_POINT ( 'NONE', #11851 ) ;
#2451 = CARTESIAN_POINT ( 'NONE',  ( -66.56242279005481066, 112.0249532631118399, 24.56082634672266707 ) ) ;
#2452 = DIRECTION ( 'NONE',  ( 0.000000000000000000, 0.000000000000000000, 1.000000000000000000 ) ) ;
#2454 = ORIENTED_EDGE ( 'NONE', *, *, #13495, .F. ) ;
#2453 = CARTESIAN_POINT ( 'NONE',  ( -76.76049879875490944, 91.67990741037235125, 63.48630363751230021 ) ) ;
#2455 = DIRECTION ( 'NONE',  ( 0.000000000000000000, 0.000000000000000000, 1.000000000000000000 ) ) ;
#2456 = AXIS2_PLACEMENT_3D ( 'NONE', #15865, #7367, #13080 ) ;
#2457 = CIRCLE ( 'NONE', #4829, 12.50000000000001776 ) ;
#2458 = DIRECTION ( 'NONE',  ( 0.000000000000000000, 0.000000000000000000, 1.000000000000000000 ) ) ;
#2459 = ORIENTED_EDGE ( 'NONE', *, *, #11119, .T. ) ;
#2460 = CYLINDRICAL_SURFACE ( 'NONE', #251, 5.000000000000000000 ) ;
#2461 = ORIENTED_EDGE ( 'NONE', *, *, #9720, .T. ) ;
#2462 = AXIS2_PLACEMENT_3D ( 'NONE', #6172, #2259, #13314 ) ;
#2463 = EDGE_LOOP ( 'NONE', ( #12801, #6878, #9677, #17977 ) ) ;
#2464 = VECTOR ( 'NONE', #14089, 1000.000000000000000 ) ;
#2465 = VECTOR ( 'NONE', #18294, 1000.000000000000000 ) ;
#2466 = CARTESIAN_POINT ( 'NONE',  ( 15.23320273812466041, -46.83756720124470263, 115.7605492041889619 ) ) ;
#2467 = DIRECTION ( 'NONE',  ( -0.000000000000000000, -0.000000000000000000, 1.000000000000000000 ) ) ;
#2468 = CYLINDRICAL_SURFACE ( 'NONE', #666, 12.50000000000001066 ) ;
#2469 = ORIENTED_EDGE ( 'NONE', *, *, #16993, .T. ) ;
#2470 = CONTEXT_DEPENDENT_SHAPE_REPRESENTATION ( #4648, #16232 ) ;
#2471 = CARTESIAN_POINT ( 'NONE',  ( -30.39988730823796104, -91.18731141006421126, 9.610196039195450624 ) ) ;
#2472 = DIRECTION ( 'NONE',  ( -0.9475106458593564041, 0.3197242186372270534, -0.000000000000000000 ) ) ;
#2473 = ORIENTED_EDGE ( 'NONE', *, *, #11659, .F. ) ;
#2474 = CIRCLE ( 'NONE', #3078, 10.38004356723770627 ) ;
#2475 = DIRECTION ( 'NONE',  ( 0.000000000000000000, 0.000000000000000000, 1.000000000000000000 ) ) ;
#2476 = CARTESIAN_POINT ( 'NONE',  ( -66.63376473465912397, -19.34983604512935429, 57.00000000000000000 ) ) ;
#2477 = LINE ( 'NONE', #8471, #11737 ) ;
#2478 = ORIENTED_EDGE ( 'NONE', *, *, #9167, .T. ) ;
#2479 = PLANE ( 'NONE',  #11044 ) ;
#2480 = LINE ( 'NONE', #13906, #3660 ) ;
#2481 = ORIENTED_EDGE ( 'NONE', *, *, #414, .T. ) ;
#2482 = VECTOR ( 'NONE', #7749, 1000.000000000000000 ) ;
#2483 = AXIS2_PLACEMENT_3D ( 'NONE', #14914, #2114, #13534 ) ;
#2484 = CARTESIAN_POINT ( 'NONE',  ( -7.840676406241780860, 112.6569076202650308, 92.50000000000000000 ) ) ;
#2485 = AXIS2_PLACEMENT_3D ( 'NONE', #10357, #14738, #15875 ) ;
#2486 = CARTESIAN_POINT ( 'NONE',  ( -57.99147934508202695, 74.02016676429184372, -167.1454815528550739 ) ) ;
#2487 = ORIENTED_EDGE ( 'NONE', *, *, #16152, .F. ) ;
#2488 = VECTOR ( 'NONE', #5761, 1000.000000000000000 ) ;
#2489 = LINE ( 'NONE', #13914, #14735 ) ;
#2490 = DIRECTION ( 'NONE',  ( 0.000000000000000000, 1.000000000000000000, -0.000000000000000000 ) ) ;
#2491 = ORIENTED_EDGE ( 'NONE', *, *, #6258, .F. ) ;
#2492 = EDGE_CURVE ( 'NONE', #12417, #10310, #7283, .T. ) ;
#2493 = VECTOR ( 'NONE', #17943, 1000.000000000000000 ) ;
#2494 = FACE_OUTER_BOUND ( 'NONE', #12973, .T. ) ;
#2496 = CIRCLE ( 'NONE', #16231, 10.24900000000001477 ) ;
#2495 = CARTESIAN_POINT ( 'NONE',  ( -57.08002265617300708, 84.22855780814606419, 25.00000000000000355 ) ) ;
#2497 = CARTESIAN_POINT ( 'NONE',  ( -46.00604326503374608, 49.61971273109995195, 27.56969510706493764 ) ) ;
#2498 = CARTESIAN_POINT ( 'NONE',  ( -107.5926225674731711, 57.88796029049330372, 30.38417033480641294 ) ) ;
#2499 = ORIENTED_EDGE ( 'NONE', *, *, #12714, .T. ) ;
#2500 = CARTESIAN_POINT ( 'NONE',  ( -68.99615306438077766, 117.6340838816626899, 15.00000000000006928 ) ) ;
#2501 = DIRECTION ( 'NONE',  ( 1.000000000000000000, 0.000000000000000000, 0.000000000000000000 ) ) ;
#2502 = CARTESIAN_POINT ( 'NONE',  ( -98.90286936182243949, -91.08423613455721579, 10.65431531532547638 ) ) ;
#2503 = APPLICATION_CONTEXT ( 'automotive_design' ) ;
#2504 = CARTESIAN_POINT ( 'NONE',  ( 4.873318353650091694, -11.10456963339436598, -53.31387177695791735 ) ) ;
#2505 = FACE_OUTER_BOUND ( 'NONE', #10827, .T. ) ;
#2506 = ORIENTED_EDGE ( 'NONE', *, *, #17580, .F. ) ;
#2507 = CARTESIAN_POINT ( 'NONE',  ( -68.99615306438083451, 102.5409764881302692, -167.1454815528550739 ) ) ;
#2508 = DIRECTION ( 'NONE',  ( -1.000000000000000000, -0.000000000000000000, -0.000000000000000000 ) ) ;
#2509 = EDGE_CURVE ( 'NONE', #11177, #6138, #6980, .T. ) ;
#2510 = FACE_OUTER_BOUND ( 'NONE', #11346, .T. ) ;
#2511 = CIRCLE ( 'NONE', #3388, 12.49999999999999112 ) ;
#2512 = VERTEX_POINT ( 'NONE', #7452 ) ;
#2513 = CIRCLE ( 'NONE', #1338, 10.24899999999999345 ) ;
#2514 = ORIENTED_EDGE ( 'NONE', *, *, #3214, .T. ) ;
#2515 = DIRECTION ( 'NONE',  ( -1.000000000000000000, -4.124608743189000987E-16, 0.000000000000000000 ) ) ;
#2516 = EDGE_CURVE ( 'NONE', #2231, #11979, #17457, .T. ) ;
#2517 = ORIENTED_EDGE ( 'NONE', *, *, #5620, .T. ) ;
#2518 = EDGE_CURVE ( 'NONE', #10461, #15190, #6209, .T. ) ;
#2519 = DIRECTION ( 'NONE',  ( -2.062304371594500494E-16, 1.000000000000000000, -0.000000000000000000 ) ) ;
#2520 = DIRECTION ( 'NONE',  ( -0.000000000000000000, -0.000000000000000000, 1.000000000000000000 ) ) ;
#2521 = CARTESIAN_POINT ( 'NONE',  ( -66.34341644926747961, 56.84031775370380046, -27.99999999999999645 ) ) ;
#2522 = ORIENTED_EDGE ( 'NONE', *, *, #8591, .T. ) ;
#2523 = VECTOR ( 'NONE', #12420, 1000.000000000000000 ) ;
#2524 = EDGE_CURVE ( 'NONE', #15955, #11788, #13632, .T. ) ;
#2525 = DIRECTION ( 'NONE',  ( 1.000000000000000000, 2.062304371594500494E-16, -0.000000000000000000 ) ) ;
#2526 = VECTOR ( 'NONE', #7508, 1000.000000000000000 ) ;
#2527 = VECTOR ( 'NONE', #14900, 1000.000000000000000 ) ;
#2528 = CARTESIAN_POINT ( 'NONE',  ( 0.01372220897661185005, 5.948365447239559067, 2.697128823393907471 ) ) ;
#2529 = DIRECTION ( 'NONE',  ( 0.9396926207859148672, 0.3420201433256507273, 4.890320548438483418E-16 ) ) ;
#2530 = CIRCLE ( 'NONE', #13002, 10.24899999999998812 ) ;
#2531 = LINE ( 'NONE', #12545, #15899 ) ;
#2532 = PRODUCT ( 'Drive Gear', 'Drive Gear', '', ( #2019 ) ) ;
#2533 = ORIENTED_EDGE ( 'NONE', *, *, #7319, .T. ) ;
#2534 = DIRECTION ( 'NONE',  ( 1.156482317317869999E-16, 0.000000000000000000, 1.000000000000000000 ) ) ;
#2535 = EDGE_CURVE ( 'NONE', #9465, #1454, #13347, .T. ) ;
#2536 = DIRECTION ( 'NONE',  ( -5.204170427930409450E-16, 0.000000000000000000, 1.000000000000000000 ) ) ;
#2537 = EDGE_CURVE ( 'NONE', #18088, #11181, #3799, .T. ) ;
#2538 = VERTEX_POINT ( 'NONE', #16607 ) ;
#2539 = EDGE_CURVE ( 'NONE', #12123, #16319, #619, .T. ) ;
#2540 = MECHANICAL_DESIGN_GEOMETRIC_PRESENTATION_REPRESENTATION (  '', ( #6710 ), #15684 ) ;
#2541 = DIRECTION ( 'NONE',  ( 0.000000000000000000, 0.000000000000000000, 1.000000000000000000 ) ) ;
#2542 = LINE ( 'NONE', #9456, #13117 ) ;
#2543 = ORIENTED_EDGE ( 'NONE', *, *, #12676, .T. ) ;
#2544 = EDGE_CURVE ( 'NONE', #6958, #8849, #1907, .T. ) ;
#2545 = ORIENTED_EDGE ( 'NONE', *, *, #2518, .T. ) ;
#2546 = VECTOR ( 'NONE', #13082, 1000.000000000000000 ) ;
#2547 = VECTOR ( 'NONE', #13470, 1000.000000000000000 ) ;
#2548 = CIRCLE ( 'NONE', #7032, 10.24899999999998812 ) ;
#2549 = VERTEX_POINT ( 'NONE', #16234 ) ;
#2550 = UNCERTAINTY_MEASURE_WITH_UNIT (LENGTH_MEASURE( 1.000000000000000082E-05 ), #13330, 'distance_accuracy_value', 'NONE');
#2551 = ADVANCED_FACE ( 'NONE', ( #15115 ), #9319, .T. ) ;
#2552 = EDGE_CURVE ( 'NONE', #14168, #3406, #1936, .T. ) ;
#2553 = DIRECTION ( 'NONE',  ( 0.000000000000000000, 0.000000000000000000, 1.000000000000000000 ) ) ;
#2554 = CYLINDRICAL_SURFACE ( 'NONE', #6659, 5.654315315325680658 ) ;
#2555 = DIRECTION ( 'NONE',  ( 0.000000000000000000, 0.000000000000000000, -1.000000000000000000 ) ) ;
#2556 = LINE ( 'NONE', #4053, #10533 ) ;
#2557 = DIRECTION ( 'NONE',  ( 1.156482317317869999E-16, 0.000000000000000000, 1.000000000000000000 ) ) ;
#2558 = DIRECTION ( 'NONE',  ( 0.9396926207859084279, 0.3420201433256686574, -1.086737899652989892E-16 ) ) ;
#2559 = ORIENTED_EDGE ( 'NONE', *, *, #6394, .T. ) ;
#2560 = CIRCLE ( 'NONE', #18079, 4.600000000000020961 ) ;
#2561 = DIRECTION ( 'NONE',  ( -0.9396926207859093161, 0.3420201433256661594, 1.086737899652990878E-16 ) ) ;
#2562 = CARTESIAN_POINT ( 'NONE',  ( -107.5926225674732137, 107.8748711238780373, 25.00000000000000000 ) ) ;
#2564 = ORIENTED_EDGE ( 'NONE', *, *, #18180, .F. ) ;
#2563 = CARTESIAN_POINT ( 'NONE',  ( -78.12361985383350316, 84.22855780814607840, 70.00000000000001421 ) ) ;
#2565 = DIRECTION ( 'NONE',  ( 0.3420201433256444545, -0.9396926207859171987, 0.000000000000000000 ) ) ;
#2566 = VECTOR ( 'NONE', #14567, 1000.000000000000000 ) ;
#2567 = CARTESIAN_POINT ( 'NONE',  ( -71.24615306438089135, 82.25763170456374951, -167.1454815528550739 ) ) ;
#2568 = ORIENTED_EDGE ( 'NONE', *, *, #1290, .T. ) ;
#2569 = CARTESIAN_POINT ( 'NONE',  ( -52.55467279550843784, 75.03273214436886462, 15.00000000000006928 ) ) ;
#2570 = ORIENTED_EDGE ( 'NONE', *, *, #678, .F. ) ;
#2571 = EDGE_CURVE ( 'NONE', #12287, #1357, #8781, .T. ) ;
#2572 = ORIENTED_EDGE ( 'NONE', *, *, #15789, .T. ) ;
#2573 = VECTOR ( 'NONE', #1278, 1000.000000000000114 ) ;
#2574 = VECTOR ( 'NONE', #18223, 1000.000000000000000 ) ;
#2575 = DIRECTION ( 'NONE',  ( 0.000000000000000000, 0.000000000000000000, 1.000000000000000000 ) ) ;
#2576 = CARTESIAN_POINT ( 'NONE',  ( -71.24615306438073503, 128.4926507152292459, -15.00000000000001421 ) ) ;
#2577 = VERTEX_POINT ( 'NONE', #5096 ) ;
#2578 = ORIENTED_EDGE ( 'NONE', *, *, #11481, .T. ) ;
#2579 = CARTESIAN_POINT ( 'NONE',  ( -36.44155368744860368, 56.74635804676025685, -22.50216374311546019 ) ) ;
#2580 = DIRECTION ( 'NONE',  ( -0.000000000000000000, 1.000000000000000000, 0.000000000000000000 ) ) ;
#2581 = VERTEX_POINT ( 'NONE', #5001 ) ;
#2582 = CARTESIAN_POINT ( 'NONE',  ( -57.08002265617300708, 84.22855780814606419, -47.49999999999999289 ) ) ;
#2583 = DIRECTION ( 'NONE',  ( 0.000000000000000000, 0.000000000000000000, 1.000000000000000000 ) ) ;
#2584 = DIRECTION ( 'NONE',  ( 0.000000000000000000, 0.000000000000000000, 1.000000000000000000 ) ) ;
#2585 = ORIENTED_EDGE ( 'NONE', *, *, #17243, .T. ) ;
#2586 = CARTESIAN_POINT ( 'NONE',  ( -57.08002265617300708, 84.22855780814606419, 35.00000000000000000 ) ) ;
#2587 = CARTESIAN_POINT ( 'NONE',  ( 97.91997734382704266, 84.22855780814606419, 62.50000000000001421 ) ) ;
#2588 = ORIENTED_EDGE ( 'NONE', *, *, #9820, .F. ) ;
#2589 = CARTESIAN_POINT ( 'NONE',  ( -54.93063083320800644, 106.4346967249107792, 97.49999999999998579 ) ) ;
#2590 = CARTESIAN_POINT ( 'NONE',  ( -68.99615306438094819, 64.22700883166265839, -15.00000000000001421 ) ) ;
#2591 = ORIENTED_EDGE ( 'NONE', *, *, #3525, .F. ) ;
#2592 = EDGE_LOOP ( 'NONE', ( #2918, #8135, #9443, #11259 ) ) ;
#2593 = ORIENTED_EDGE ( 'NONE', *, *, #15561, .F. ) ;
#2594 = DIRECTION ( 'NONE',  ( -1.224646799147353207E-16, 1.000000000000000000, 0.000000000000000000 ) ) ;
#2595 = DIRECTION ( 'NONE',  ( 0.000000000000000000, -1.000000000000000000, 0.000000000000000000 ) ) ;
#2596 = EDGE_LOOP ( 'NONE', ( #4401, #6883, #8878, #2682 ) ) ;
#2597 = DIRECTION ( 'NONE',  ( -0.000000000000000000, -0.000000000000000000, -1.000000000000000000 ) ) ;
#2598 = CARTESIAN_POINT ( 'NONE',  ( -68.99615306438077766, 111.3508985816626335, -167.1454815528550739 ) ) ;
#2599 = DIRECTION ( 'NONE',  ( -1.000000000000000000, 0.000000000000000000, 0.000000000000000000 ) ) ;
#2600 = DIRECTION ( 'NONE',  ( 0.000000000000000000, 0.000000000000000000, -1.000000000000000000 ) ) ;
#2601 = ORIENTED_EDGE ( 'NONE', *, *, #560, .F. ) ;
#2602 = ADVANCED_FACE ( 'NONE', ( #12038 ), #10813, .T. ) ;
#2603 = CARTESIAN_POINT ( 'NONE',  ( -71.24615306438080609, 109.6430948152292189, 15.00000000000006928 ) ) ;
#2604 = DIRECTION ( 'NONE',  ( -5.204170427930409450E-16, 0.000000000000000000, 1.000000000000000000 ) ) ;
#2605 = LINE ( 'NONE', #1112, #15405 ) ;
#2606 = CARTESIAN_POINT ( 'NONE',  ( -42.53669312409158465, -111.0842361345572158, -5.654315315325675328 ) ) ;
#2607 = FACE_OUTER_BOUND ( 'NONE', #13874, .T. ) ;
#2608 = EDGE_LOOP ( 'NONE', ( #4885, #10142, #8906, #11620 ) ) ;
#2609 = DIRECTION ( 'NONE',  ( 0.000000000000000000, 1.000000000000000000, 0.000000000000000000 ) ) ;
#2610 = CARTESIAN_POINT ( 'NONE',  ( -68.99615306438072082, 130.2004544816626890, 15.00000000000006928 ) ) ;
#2611 = DIRECTION ( 'NONE',  ( -0.9396926207859069846, 0.3420201433256723766, -4.890320548438442003E-16 ) ) ;
#2612 = CARTESIAN_POINT ( 'NONE',  ( -36.37443156682203949, 80.46558623543624833, 68.99235718476280965 ) ) ;
#2613 = VERTEX_POINT ( 'NONE', #18013 ) ;
#2614 = ORIENTED_EDGE ( 'NONE', *, *, #1969, .F. ) ;
#2615 = LINE ( 'NONE', #8313, #6675 ) ;
#2616 = ORIENTED_EDGE ( 'NONE', *, *, #11228, .F. ) ;
#2617 = LINE ( 'NONE', #2419, #174 ) ;
#2618 = DIRECTION ( 'NONE',  ( 0.000000000000000000, -1.000000000000000000, 0.000000000000000000 ) ) ;
#2619 = DIRECTION ( 'NONE',  ( 1.000000000000000000, 2.062304371594500494E-16, -0.000000000000000000 ) ) ;
#2620 = ORIENTED_EDGE ( 'NONE', *, *, #11343, .T. ) ;
#2621 = EDGE_CURVE ( 'NONE', #15787, #14076, #16508, .T. ) ;
#2622 = DIRECTION ( 'NONE',  ( -1.000000000000000000, 0.000000000000000000, 0.000000000000000000 ) ) ;
#2623 = DIRECTION ( 'NONE',  ( 1.000000000000000000, 0.000000000000000000, 0.000000000000000000 ) ) ;
#2624 = CARTESIAN_POINT ( 'NONE',  ( -57.08002265617300708, 84.22855780814606419, 15.00000000000006928 ) ) ;
#2625 = ORIENTED_EDGE ( 'NONE', *, *, #14181, .F. ) ;
#2626 = FACE_OUTER_BOUND ( 'NONE', #17993, .T. ) ;
#2627 = ORIENTED_EDGE ( 'NONE', *, *, #12477, .F. ) ;
#2628 = EDGE_CURVE ( 'NONE', #4375, #9885, #17739, .T. ) ;
#2629 = FACE_OUTER_BOUND ( 'NONE', #18193, .T. ) ;
#2630 = CARTESIAN_POINT ( 'NONE',  ( -68.99615306438077766, 111.3508985816626335, -15.00000000000001421 ) ) ;
#2631 = ORIENTED_EDGE ( 'NONE', *, *, #3655, .T. ) ;
#2632 = ORIENTED_EDGE ( 'NONE', *, *, #15806, .T. ) ;
#2633 = VERTEX_POINT ( 'NONE', #9140 ) ;
#2634 = ADVANCED_FACE ( 'NONE', ( #14828 ), #13432, .T. ) ;
#2635 = LINE ( 'NONE', #3841, #436 ) ;
#2636 = DIRECTION ( 'NONE',  ( 0.000000000000000000, 0.000000000000000000, 1.000000000000000000 ) ) ;
#2637 = EDGE_CURVE ( 'NONE', #3659, #616, #2496, .T. ) ;
#2638 = CARTESIAN_POINT ( 'NONE',  ( -38.09490121289055509, 73.26749283227019305, 97.49999999999998579 ) ) ;
#2639 = PLANE ( 'NONE',  #6340 ) ;
#2640 = EDGE_CURVE ( 'NONE', #11938, #13177, #7818, .T. ) ;
#2641 = CARTESIAN_POINT ( 'NONE',  ( -50.81952187608693805, 73.40930968350535579, -167.1454815528550739 ) ) ;
#2642 = DIRECTION ( 'NONE',  ( 0.000000000000000000, 0.000000000000000000, 1.000000000000000000 ) ) ;
#2643 = ORIENTED_EDGE ( 'NONE', *, *, #5496, .T. ) ;
#2644 = FACE_OUTER_BOUND ( 'NONE', #12760, .T. ) ;
#2645 = ORIENTED_EDGE ( 'NONE', *, *, #12131, .T. ) ;
#2646 = DIRECTION ( 'NONE',  ( -1.000000000000000000, -1.218656359355351063E-14, 1.692578276882432005E-16 ) ) ;
#2647 = LINE ( 'NONE', #9766, #8665 ) ;
#2648 = VECTOR ( 'NONE', #7974, 1000.000000000000114 ) ;
#2649 = EDGE_LOOP ( 'NONE', ( #3464, #7315, #8248, #10385 ) ) ;
#2650 = EDGE_CURVE ( 'NONE', #3838, #3665, #16533, .T. ) ;
#2651 = EDGE_CURVE ( 'NONE', #8001, #17304, #2207, .T. ) ;
#2652 = EDGE_CURVE ( 'NONE', #2688, #14160, #2489, .T. ) ;
#2653 = FACE_OUTER_BOUND ( 'NONE', #13653, .T. ) ;
#2654 = ORIENTED_EDGE ( 'NONE', *, *, #1622, .T. ) ;
#2655 = EDGE_CURVE ( 'NONE', #9500, #14160, #708, .T. ) ;
#2656 = ORIENTED_EDGE ( 'NONE', *, *, #3673, .F. ) ;
#2657 = EDGE_CURVE ( 'NONE', #17012, #4505, #3991, .T. ) ;
#2658 = VECTOR ( 'NONE', #563, 1000.000000000000000 ) ;
#2659 = CARTESIAN_POINT ( 'NONE',  ( -71.24615306438090556, 63.40807580456378645, 15.00000000000006928 ) ) ;
#2660 = DIRECTION ( 'NONE',  ( 0.000000000000000000, 0.000000000000000000, 1.000000000000000000 ) ) ;
#2661 = ORIENTED_EDGE ( 'NONE', *, *, #12027, .F. ) ;
#2662 = ORIENTED_EDGE ( 'NONE', *, *, #7620, .F. ) ;
#2663 = ADVANCED_FACE ( 'NONE', ( #6795 ), #13556, .T. ) ;
#2664 = DIRECTION ( 'NONE',  ( 0.000000000000000000, 1.000000000000000000, 0.000000000000000000 ) ) ;
#2665 = EDGE_CURVE ( 'NONE', #13490, #2052, #17722, .T. ) ;
#2666 = LINE ( 'NONE', #15391, #749 ) ;
#2667 = ORIENTED_EDGE ( 'NONE', *, *, #7976, .T. ) ;
#2668 = PLANE ( 'NONE',  #14664 ) ;
#2669 = DIRECTION ( 'NONE',  ( -0.000000000000000000, -0.000000000000000000, -1.000000000000000000 ) ) ;
#2670 = ORIENTED_EDGE ( 'NONE', *, *, #14218, .T. ) ;
#2671 = PLANE ( 'NONE',  #15226 ) ;
#2672 = DIRECTION ( 'NONE',  ( -1.000000000000000000, -2.062304371594500247E-16, -0.000000000000000000 ) ) ;
#2673 = EDGE_LOOP ( 'NONE', ( #4761, #12857, #12685, #17857, #9212 ) ) ;
#2674 = DIRECTION ( 'NONE',  ( 1.000000000000000000, -0.000000000000000000, -0.000000000000000000 ) ) ;
#2675 = AXIS2_PLACEMENT_3D ( 'NONE', #15951, #17437, #6110 ) ;
#2676 = CARTESIAN_POINT ( 'NONE',  ( -92.59262256747319952, 57.88796029049329661, 26.35917033480641436 ) ) ;
#2677 = ORIENTED_EDGE ( 'NONE', *, *, #7820, .T. ) ;
#2678 = B_SPLINE_CURVE_WITH_KNOTS ( 'NONE', 3,
 ( #5562, #5465, #13995, #1175 ),
 .UNSPECIFIED., .F., .F.,
 ( 4, 4 ),
 ( 0.007714237994431366770, 0.01042320952183839987 ),
 .UNSPECIFIED. ) ;
#2679 = PRODUCT ( 'Plastic-Ended Handle', 'Plastic-Ended Handle', '', ( #6865 ) ) ;
#2680 = CARTESIAN_POINT ( 'NONE',  ( 45.30000000000000426, 2.306883830789244121E-16, -3.445500000000021767 ) ) ;
#2681 = CARTESIAN_POINT ( 'NONE',  ( -68.99615306438100504, 45.99230878813026635, -15.00000000000001421 ) ) ;
#2682 = ORIENTED_EDGE ( 'NONE', *, *, #17075, .F. ) ;
#2683 = LINE ( 'NONE', #8202, #17588 ) ;
#2684 = DIRECTION ( 'NONE',  ( -0.000000000000000000, -0.000000000000000000, -1.000000000000000000 ) ) ;
#2685 = CARTESIAN_POINT ( 'NONE',  ( -68.99615306438077766, 124.5321250381302747, 15.00000000000006928 ) ) ;
#2686 = AXIS2_PLACEMENT_3D ( 'NONE', #12788, #5747, #12874 ) ;
#2687 = CARTESIAN_POINT ( 'NONE',  ( -57.08002265617300708, 84.22855780814606419, -35.00000000000000000 ) ) ;
#2688 = VERTEX_POINT ( 'NONE', #6701 ) ;
#2689 = CARTESIAN_POINT ( 'NONE',  ( -68.99615306438113294, -1.131580961869758761, 15.00000000000006928 ) ) ;
#2690 = CIRCLE ( 'NONE', #11362, 3.999999999999996447 ) ;
#2691 = DIRECTION ( 'NONE',  ( -1.000000000000000000, 0.000000000000000000, -4.029365176583844474E-15 ) ) ;
#2692 = FACE_OUTER_BOUND ( 'NONE', #4779, .T. ) ;
#2693 = LINE ( 'NONE', #6714, #365 ) ;
#2694 = PLANE ( 'NONE',  #5736 ) ;
#2695 = ORIENTED_EDGE ( 'NONE', *, *, #2298, .T. ) ;
#2696 = CARTESIAN_POINT ( 'NONE',  ( -57.08002265617300708, 84.22855780814606419, -167.1454815528550739 ) ) ;
#2697 = DIRECTION ( 'NONE',  ( -0.9396926207859103153, 0.3420201433256635504, 1.086737899652991987E-16 ) ) ;
#2698 = DIRECTION ( 'NONE',  ( 0.000000000000000000, 0.000000000000000000, 1.000000000000000000 ) ) ;
#2699 = DIRECTION ( 'NONE',  ( 1.000000000000000000, 0.000000000000000000, 0.000000000000000000 ) ) ;
#2700 = ORIENTED_EDGE ( 'NONE', *, *, #17709, .F. ) ;
#2701 = AXIS2_PLACEMENT_3D ( 'NONE', #14597, #10673, #557 ) ;
#2702 = ADVANCED_FACE ( 'NONE', ( #7084 ), #11104, .T. ) ;
#2703 = VERTEX_POINT ( 'NONE', #15409 ) ;
#2704 = AXIS2_PLACEMENT_3D ( 'NONE', #12165, #13845, #11966 ) ;
#2705 = FACE_OUTER_BOUND ( 'NONE', #1326, .T. ) ;
#2706 = EDGE_CURVE ( 'NONE', #9223, #4742, #10864, .T. ) ;
#2707 = ORIENTED_EDGE ( 'NONE', *, *, #2868, .F. ) ;
#2708 = DIRECTION ( 'NONE',  ( 1.000000000000000000, 0.000000000000000000, 0.000000000000000000 ) ) ;
#2709 = CARTESIAN_POINT ( 'NONE',  ( 95.45835937779679625, 56.41207303426869402, 7.000000000000010658 ) ) ;
#2710 = CARTESIAN_POINT ( 'NONE',  ( -92.59262256747321373, 110.5691553257988460, 26.35917033480641436 ) ) ;
#2711 = ORIENTED_EDGE ( 'NONE', *, *, #5283, .T. ) ;
#2712 = AXIS2_PLACEMENT_3D ( 'NONE', #640, #4570, #3346 ) ;
#2713 = CARTESIAN_POINT ( 'NONE',  ( -66.85187407874441590, 108.3380026262840090, -27.99999999999999645 ) ) ;
#2714 = LINE ( 'NONE', #1038, #14992 ) ;
#2715 = EDGE_LOOP ( 'NONE', ( #920, #6973, #18155, #7405 ) ) ;
#2716 = VECTOR ( 'NONE', #9067, 1000.000000000000000 ) ;
#2717 = AXIS2_PLACEMENT_3D ( 'NONE', #2121, #818, #7930 ) ;
#2718 = AXIS2_PLACEMENT_3D ( 'NONE', #8535, #6930, #14242 ) ;
#2719 = DIRECTION ( 'NONE',  ( 1.000000000000000000, 0.000000000000000000, 0.000000000000000000 ) ) ;
#2720 = ORIENTED_EDGE ( 'NONE', *, *, #4266, .F. ) ;
#2721 = DIRECTION ( 'NONE',  ( -1.000000000000000000, -0.000000000000000000, -0.000000000000000000 ) ) ;
#2722 = DIRECTION ( 'NONE',  ( 0.000000000000000000, 0.000000000000000000, 1.000000000000000000 ) ) ;
#2723 = ORIENTED_EDGE ( 'NONE', *, *, #6624, .F. ) ;
#2724 = ORIENTED_EDGE ( 'NONE', *, *, #13713, .T. ) ;
#2725 = VECTOR ( 'NONE', #8469, 1000.000000000000000 ) ;
#2726 = ORIENTED_EDGE ( 'NONE', *, *, #1275, .F. ) ;
#2727 = VECTOR ( 'NONE', #12412, 1000.000000000000000 ) ;
#2728 = VECTOR ( 'NONE', #13517, 1000.000000000000000 ) ;
#2729 = CARTESIAN_POINT ( 'NONE',  ( -67.59262256747317110, 56.80567558672318995, -22.50837044127973030 ) ) ;
#2730 = DIRECTION ( 'NONE',  ( 0.000000000000000000, 1.000000000000000000, 0.000000000000000000 ) ) ;
#2731 = LINE ( 'NONE', #15906, #15205 ) ;
#2732 = EDGE_CURVE ( 'NONE', #4878, #17628, #3984, .T. ) ;
#2733 = CARTESIAN_POINT ( 'NONE',  ( -65.17806329749801364, 93.75072866207683830, -15.00000000000001243 ) ) ;
#2734 = CARTESIAN_POINT ( 'NONE',  ( 0.5805565836007747782, -7.505553499465293932, 1.040834085586084257E-14 ) ) ;
#2735 = ORIENTED_EDGE ( 'NONE', *, *, #13485, .F. ) ;
#2736 = CARTESIAN_POINT ( 'NONE',  ( -97.59262256747318531, 61.64996188551983636, 25.00000000000000000 ) ) ;
#2737 = VERTEX_POINT ( 'NONE', #18409 ) ;
#2738 =( GEOMETRIC_REPRESENTATION_CONTEXT ( 3 ) GLOBAL_UNCERTAINTY_ASSIGNED_CONTEXT ( ( #1058 ) ) GLOBAL_UNIT_ASSIGNED_CONTEXT ( ( #12203, #9578, #17895 ) ) REPRESENTATION_CONTEXT ( 'NONE', 'WORKASPACE' ) );
#2739 = FACE_OUTER_BOUND ( 'NONE', #17231, .T. ) ;
#2740 = CARTESIAN_POINT ( 'NONE',  ( 105.4583593777967963, -32.62665103886256190, 7.000000000000010658 ) ) ;
#2741 = ORIENTED_EDGE ( 'NONE', *, *, #297, .F. ) ;
#2742 = AXIS2_PLACEMENT_3D ( 'NONE', #1450, #7153, #12870 ) ;
#2743 = AXIS2_PLACEMENT_3D ( 'NONE', #13147, #4441, #5857 ) ;
#2744 = CARTESIAN_POINT ( 'NONE',  ( -115.7073899772185257, -95.23217669033341792, -5.709860480175484199 ) ) ;
#2745 = ORIENTED_EDGE ( 'NONE', *, *, #11252, .F. ) ;
#2746 = EDGE_CURVE ( 'NONE', #5564, #15197, #8172, .T. ) ;
#2747 = EDGE_LOOP ( 'NONE', ( #8359, #11367 ) ) ;
#2748 = CIRCLE ( 'NONE', #944, 4.599999999999999645 ) ;
#2749 = DIRECTION ( 'NONE',  ( 0.000000000000000000, 0.000000000000000000, -1.000000000000000000 ) ) ;
#2750 = DIRECTION ( 'NONE',  ( -0.9396926207859084279, 0.3420201433256686574, 0.000000000000000000 ) ) ;
#2751 = DIRECTION ( 'NONE',  ( 0.000000000000000000, 0.000000000000000000, 1.000000000000000000 ) ) ;
#2752 = EDGE_CURVE ( 'NONE', #6089, #14417, #16984, .T. ) ;
#2753 = ORIENTED_EDGE ( 'NONE', *, *, #15986, .F. ) ;
#2754 = CONTEXT_DEPENDENT_SHAPE_REPRESENTATION ( #11364, #2356 ) ;
#2755 = EDGE_CURVE ( 'NONE', #646, #8947, #7522, .T. ) ;
#2756 = CIRCLE ( 'NONE', #9624, 3.999999999999982681 ) ;
#2757 = ORIENTED_EDGE ( 'NONE', *, *, #11242, .T. ) ;
#2758 = VECTOR ( 'NONE', #4406, 1000.000000000000000 ) ;
#2759 = CARTESIAN_POINT ( 'NONE',  ( 7.757986314337494527, 14.88675170491334221, -45.60895101101229443 ) ) ;
#2760 = CARTESIAN_POINT ( 'NONE',  ( -57.08002265617300708, 84.22855780814606419, -35.00000000000000711 ) ) ;
#2761 = ORIENTED_EDGE ( 'NONE', *, *, #1627, .T. ) ;
#2762 = DIRECTION ( 'NONE',  ( 1.000000000000000000, 0.000000000000000000, 0.000000000000000000 ) ) ;
#2763 = CARTESIAN_POINT ( 'NONE',  ( -70.71978124295668522, -96.08423613455721579, -22.52877280353970235 ) ) ;
#2764 = CARTESIAN_POINT ( 'NONE',  ( 124.5381772159375942, -151.5628872026272802, 57.00000000000000000 ) ) ;
#2765 = ORIENTED_EDGE ( 'NONE', *, *, #16546, .F. ) ;
#2766 = CARTESIAN_POINT ( 'NONE',  ( -68.99615306438087714, 55.41708673813025854, 15.00000000000006928 ) ) ;
#2767 = LINE ( 'NONE', #6788, #15308 ) ;
#2768 = VERTEX_POINT ( 'NONE', #10241 ) ;
#2769 = ADVANCED_FACE ( 'NONE', ( #6107 ), #15854, .F. ) ;
#2770 = VECTOR ( 'NONE', #10254, 1000.000000000000000 ) ;
#2771 = CARTESIAN_POINT ( 'NONE',  ( 84.41679105416972106, 84.22855780814606419, 62.50000000000001421 ) ) ;
#2772 = ORIENTED_EDGE ( 'NONE', *, *, #939, .F. ) ;
#2773 = ADVANCED_FACE ( 'NONE', ( #15695, #319 ), #5922, .T. ) ;
#2774 = LINE ( 'NONE', #2869, #9746 ) ;
#2775 = AXIS2_PLACEMENT_3D ( 'NONE', #11927, #10522, #14821 ) ;
#2776 = VECTOR ( 'NONE', #1220, 1000.000000000000000 ) ;
#2777 = ORIENTED_EDGE ( 'NONE', *, *, #6152, .T. ) ;
#2778 = EDGE_CURVE ( 'NONE', #15227, #15032, #7428, .T. ) ;
#2779 = ADVANCED_FACE ( 'NONE', ( #4363 ), #10068, .T. ) ;
#2780 = ORIENTED_EDGE ( 'NONE', *, *, #9396, .T. ) ;
#2781 = CARTESIAN_POINT ( 'NONE',  ( -48.74405704658271077, 91.10542963993684396, -167.1454815528550739 ) ) ;
#2782 = CARTESIAN_POINT ( 'NONE',  ( -71.24615306438117557, 3.717815454563750954, -167.1454815528550739 ) ) ;
#2783 = CARTESIAN_POINT ( 'NONE',  ( 4.699999999999995737, 0.000000000000000000, 0.000000000000000000 ) ) ;
#2784 = EDGE_CURVE ( 'NONE', #9825, #13777, #7258, .T. ) ;
#2785 = VECTOR ( 'NONE', #16964, 1000.000000000000000 ) ;
#2786 = VERTEX_POINT ( 'NONE', #595 ) ;
#2787 = CARTESIAN_POINT ( 'NONE',  ( -57.08002265617300708, 84.22855780814606419, 28.00000000000000355 ) ) ;
#2788 = DIRECTION ( 'NONE',  ( 1.000000000000000000, 0.000000000000000000, 0.000000000000000000 ) ) ;
#2789 = LINE ( 'NONE', #5387, #4291 ) ;
#2790 = LINE ( 'NONE', #7090, #11775 ) ;
#2791 = VERTEX_POINT ( 'NONE', #17889 ) ;
#2792 = LINE ( 'NONE', #5391, #9581 ) ;
#2793 = VECTOR ( 'NONE', #11700, 1000.000000000000000 ) ;
#2794 = VECTOR ( 'NONE', #12786, 1000.000000000000000 ) ;
#2795 = DIRECTION ( 'NONE',  ( 0.000000000000000000, 0.000000000000000000, -1.000000000000000000 ) ) ;
#2796 = CYLINDRICAL_SURFACE ( 'NONE', #967, 12.50000000000000355 ) ;
#2797 = VERTEX_POINT ( 'NONE', #10792 ) ;
#2798 = CARTESIAN_POINT ( 'NONE',  ( -68.99615306438106188, 26.52789703166272162, 15.00000000000006928 ) ) ;
#2799 = CARTESIAN_POINT ( 'NONE',  ( -71.24615306438120399, 0.5762228045637918239, -167.1454815528550739 ) ) ;
#2800 = VECTOR ( 'NONE', #9652, 1000.000000000000000 ) ;
#2801 = DIRECTION ( 'NONE',  ( 0.000000000000000000, 1.000000000000000000, 0.000000000000000000 ) ) ;
#2802 = CARTESIAN_POINT ( 'NONE',  ( -47.02742034342072941, 91.65790412808885890, -167.1454815528550739 ) ) ;
#2803 = ORIENTED_EDGE ( 'NONE', *, *, #7483, .F. ) ;
#2804 = ORIENTED_EDGE ( 'NONE', *, *, #17315, .T. ) ;
#2805 = VECTOR ( 'NONE', #1142, 1000.000000000000000 ) ;
#2806 = AXIS2_PLACEMENT_3D ( 'NONE', #15914, #3105, #8818 ) ;
#2807 = CIRCLE ( 'NONE', #10544, 12.50000000000000355 ) ;
#2808 = CARTESIAN_POINT ( 'NONE',  ( 0.1061556211656219523, -6.421950209808431786, -1.876855952934466387 ) ) ;
#2809 = VERTEX_POINT ( 'NONE', #3685 ) ;
#2810 = CARTESIAN_POINT ( 'NONE',  ( -68.99615306438074924, 120.7756765316626542, 15.00000000000006928 ) ) ;
#2811 = CARTESIAN_POINT ( 'NONE',  ( -68.43628269749412141, 111.3280217493016266, -22.41747227276117727 ) ) ;
#2812 = ORIENTED_EDGE ( 'NONE', *, *, #7926, .T. ) ;
#2813 = VECTOR ( 'NONE', #16740, 1000.000000000000000 ) ;
#2814 = CARTESIAN_POINT ( 'NONE',  ( -66.20572860746047184, 111.1782190889722983, -28.00000000000000355 ) ) ;
#2815 = CARTESIAN_POINT ( 'NONE',  ( -46.03642545851250389, 84.22855780814606419, -47.50000000000000000 ) ) ;
#2816 = CARTESIAN_POINT ( 'NONE',  ( 124.5381772159375942, -111.0842361345572158, 57.00000000000000000 ) ) ;
#2817 = CARTESIAN_POINT ( 'NONE',  ( -68.99615306438111872, 7.678341131662685726, -167.1454815528550739 ) ) ;
#2818 = EDGE_LOOP ( 'NONE', ( #6948, #15133, #122, #13825, #10648, #488 ) ) ;
#2819 =( GEOMETRIC_REPRESENTATION_CONTEXT ( 3 ) GLOBAL_UNCERTAINTY_ASSIGNED_CONTEXT ( ( #16559 ) ) GLOBAL_UNIT_ASSIGNED_CONTEXT ( ( #443, #14568, #5870 ) ) REPRESENTATION_CONTEXT ( 'NONE', 'WORKASPACE' ) );
#2820 = CIRCLE ( 'NONE', #6674, 5.654315315325680658 ) ;
#2821 = VECTOR ( 'NONE', #4174, 1000.000000000000000 ) ;
#2822 = DIRECTION ( 'NONE',  ( 0.3420201433256649937, -0.9396926207859097602, 0.000000000000000000 ) ) ;
#2823 = ORIENTED_EDGE ( 'NONE', *, *, #10499, .T. ) ;
#2824 = DIRECTION ( 'NONE',  ( 0.000000000000000000, 0.000000000000000000, 1.000000000000000000 ) ) ;
#2825 = DIRECTION ( 'NONE',  ( 0.000000000000000000, 1.000000000000000000, 0.000000000000000000 ) ) ;
#2826 = ORIENTED_EDGE ( 'NONE', *, *, #14984, .T. ) ;
#2827 = EDGE_LOOP ( 'NONE', ( #16884, #5507, #2478, #6522 ) ) ;
#2828 = MECHANICAL_DESIGN_GEOMETRIC_PRESENTATION_REPRESENTATION (  '', ( #10581 ), #5497 ) ;
#2829 = ORIENTED_EDGE ( 'NONE', *, *, #13086, .T. ) ;
#2830 = VECTOR ( 'NONE', #1846, 1000.000000000000000 ) ;
#2831 = AXIS2_PLACEMENT_3D ( 'NONE', #1623, #11550, #5904 ) ;
#2832 = DIRECTION ( 'NONE',  ( 0.9396926207859171987, 0.3420201433256444545, 0.000000000000000000 ) ) ;
#2833 = CARTESIAN_POINT ( 'NONE',  ( -71.24615306438070661, 141.9478920545637664, 15.00000000000006928 ) ) ;
#2834 = CARTESIAN_POINT ( 'NONE',  ( -79.12361985383350316, 84.22855780814606419, -124.8487082408420861 ) ) ;
#2835 = CARTESIAN_POINT ( 'NONE',  ( -67.59262256747317110, 61.53592931583062153, -28.00000000000000355 ) ) ;
#2836 = CARTESIAN_POINT ( 'NONE',  ( -57.99147934508202695, 74.02016676429184372, -15.00000000000001421 ) ) ;
#2837 = VERTEX_POINT ( 'NONE', #9397 ) ;
#2838 = EDGE_CURVE ( 'NONE', #9739, #15151, #17147, .T. ) ;
#2839 = CIRCLE ( 'NONE', #13284, 10.04359719766049430 ) ;
#2840 = CARTESIAN_POINT ( 'NONE',  ( 3.930119462001817841E-14, -111.0842361345572158, -5.654315315325195712 ) ) ;
#2841 = ORIENTED_EDGE ( 'NONE', *, *, #16008, .F. ) ;
#2842 = CARTESIAN_POINT ( 'NONE',  ( -68.99615306438089135, 83.07656473166271383, -167.1454815528550739 ) ) ;
#2843 = CARTESIAN_POINT ( 'NONE',  ( -71.24615306438120399, 0.5762228045637918239, -167.1454815528550739 ) ) ;
#2844 = ORIENTED_EDGE ( 'NONE', *, *, #3221, .F. ) ;
#2845 = VECTOR ( 'NONE', #10436, 1000.000000000000000 ) ;
#2846 = VECTOR ( 'NONE', #7707, 1000.000000000000000 ) ;
#2847 = CARTESIAN_POINT ( 'NONE',  ( -57.08002265617300708, 84.22855780814606419, -61.50000000000000000 ) ) ;
#2849 = ORIENTED_EDGE ( 'NONE', *, *, #10335, .F. ) ;
#2848 = VECTOR ( 'NONE', #8624, 1000.000000000000000 ) ;
#2850 = EDGE_LOOP ( 'NONE', ( #5631, #7903, #1550, #6173 ) ) ;
#2851 = FACE_OUTER_BOUND ( 'NONE', #16830, .T. ) ;
#2852 = CARTESIAN_POINT ( 'NONE',  ( -76.37409655828280108, -91.08423613455721579, 45.05044770573179846 ) ) ;
#2853 = AXIS2_PLACEMENT_3D ( 'NONE', #16279, #3469, #10214 ) ;
#2854 = ORIENTED_EDGE ( 'NONE', *, *, #4143, .F. ) ;
#2855 = VERTEX_POINT ( 'NONE', #18281 ) ;
#2856 = VECTOR ( 'NONE', #6153, 1000.000000000000000 ) ;
#2857 = CIRCLE ( 'NONE', #13026, 6.500000000000039968 ) ;
#2858 = CARTESIAN_POINT ( 'NONE',  ( 14.89901151198486495, -10.87016367198019040, -53.26726757078508712 ) ) ;
#2859 = CARTESIAN_POINT ( 'NONE',  ( -107.5926225674731995, 60.58224449241411946, 35.00000000000000000 ) ) ;
#2860 = ORIENTED_EDGE ( 'NONE', *, *, #18204, .T. ) ;
#2861 = CARTESIAN_POINT ( 'NONE',  ( -57.08002265617300708, 84.22855780814606419, -28.00000000000000355 ) ) ;
#2862 = DIRECTION ( 'NONE',  ( -1.000000000000000000, -6.661338147750943976E-15, 1.387778780781446662E-16 ) ) ;
#2863 = ADVANCED_FACE ( 'NONE', ( #12494 ), #8175, .T. ) ;
#2864 = PLANE ( 'NONE',  #12332 ) ;
#2865 = ORIENTED_EDGE ( 'NONE', *, *, #15817, .F. ) ;
#2866 = DIRECTION ( 'NONE',  ( 2.062304371594500740E-16, -1.000000000000000000, 0.000000000000000000 ) ) ;
#2867 = VERTEX_POINT ( 'NONE', #5554 ) ;
#2868 = EDGE_CURVE ( 'NONE', #9420, #10261, #5487, .T. ) ;
#2869 = CARTESIAN_POINT ( 'NONE',  ( -68.99615306438063556, 137.0984956381302879, 15.00000000000006928 ) ) ;
#2870 = VECTOR ( 'NONE', #17921, 1000.000000000000000 ) ;
#2871 = EDGE_LOOP ( 'NONE', ( #12399, #16730, #1652, #15681 ) ) ;
#2872 = AXIS2_PLACEMENT_3D ( 'NONE', #13058, #223, #8747 ) ;
#2873 = VERTEX_POINT ( 'NONE', #11179 ) ;
#2874 = EDGE_CURVE ( 'NONE', #6902, #11029, #5178, .T. ) ;
#2875 = DIRECTION ( 'NONE',  ( 1.000000000000000000, 0.000000000000000000, 0.000000000000000000 ) ) ;
#2876 = DIRECTION ( 'NONE',  ( -1.000000000000000000, -0.000000000000000000, -0.000000000000000000 ) ) ;
#2877 = EDGE_LOOP ( 'NONE', ( #11890, #16937, #6354 ) ) ;
#2878 = ADVANCED_FACE ( 'NONE', ( #6861 ), #16667, .T. ) ;
#2879 = CARTESIAN_POINT ( 'NONE',  ( -67.59262256747317110, 57.88796029049329661, 26.35917033480641436 ) ) ;
#2880 = CARTESIAN_POINT ( 'NONE',  ( -57.08002265617300708, 84.22855780814606419, -15.00000000000001421 ) ) ;
#2881 = DIRECTION ( 'NONE',  ( 0.000000000000000000, 1.000000000000000000, 0.000000000000000000 ) ) ;
#2882 = ADVANCED_FACE ( 'NONE', ( #18185 ), #976, .T. ) ;
#2883 = CARTESIAN_POINT ( 'NONE',  ( -102.5926225674731853, 102.8748711238780373, -20.00000000000000355 ) ) ;
#2884 = VERTEX_POINT ( 'NONE', #18098 ) ;
#2885 = ADVANCED_FACE ( 'NONE', ( #15278 ), #4071, .T. ) ;
#2886 = CARTESIAN_POINT ( 'NONE',  ( -71.24615306438109030, 25.70896400456376796, -15.00000000000001421 ) ) ;
#2887 = LINE ( 'NONE', #4446, #5435 ) ;
#2888 = CARTESIAN_POINT ( 'NONE',  ( 10.78766931562283737, 7.280728192202457372, 48.30793737034424140 ) ) ;
#2889 = VERTEX_POINT ( 'NONE', #5352 ) ;
#2890 = DIRECTION ( 'NONE',  ( -1.000000000000000000, 0.000000000000000000, 0.000000000000000000 ) ) ;
#2891 = FACE_OUTER_BOUND ( 'NONE', #13092, .T. ) ;
#2892 = EDGE_CURVE ( 'NONE', #6902, #6728, #1165, .T. ) ;
#2893 = ADVANCED_FACE ( 'NONE', ( #5274 ), #16765, .T. ) ;
#2894 = DIRECTION ( 'NONE',  ( 1.000000000000000000, 0.000000000000000000, 0.000000000000000000 ) ) ;
#2895 = EDGE_CURVE ( 'NONE', #6955, #10161, #6962, .T. ) ;
#2896 = DIRECTION ( 'NONE',  ( -0.9396926207859068736, 0.3420201433256726542, 0.000000000000000000 ) ) ;
#2897 = ORIENTED_EDGE ( 'NONE', *, *, #2784, .T. ) ;
#2898 = ORIENTED_EDGE ( 'NONE', *, *, #3063, .T. ) ;
#2899 = EDGE_CURVE ( 'NONE', #4662, #14342, #16588, .T. ) ;
#2900 = DIRECTION ( 'NONE',  ( 0.3420201433256701007, -0.9396926207859078728, 0.000000000000000000 ) ) ;
#2901 = ORIENTED_EDGE ( 'NONE', *, *, #8952, .T. ) ;
#2902 = CARTESIAN_POINT ( 'NONE',  ( -67.59262256747319952, 111.6514400295689171, -22.50837044127971254 ) ) ;
#2903 = DIRECTION ( 'NONE',  ( 0.000000000000000000, 0.000000000000000000, 1.000000000000000000 ) ) ;
#2904 = CARTESIAN_POINT ( 'NONE',  ( -60.32591256472567665, -91.08930925317537231, -39.31392926885246197 ) ) ;
#2905 = ORIENTED_EDGE ( 'NONE', *, *, #9161, .T. ) ;
#2906 = LINE ( 'NONE', #8526, #4764 ) ;
#2907 = FACE_OUTER_BOUND ( 'NONE', #6040, .T. ) ;
#2908 = EDGE_CURVE ( 'NONE', #14911, #6285, #14073, .T. ) ;
#2909 = CARTESIAN_POINT ( 'NONE',  ( -57.08002265617300708, 84.22855780814606419, -167.1454815528550739 ) ) ;
#2910 = ORIENTED_EDGE ( 'NONE', *, *, #14027, .F. ) ;
#2911 = EDGE_CURVE ( 'NONE', #15151, #8454, #17991, .T. ) ;
#2912 = LINE ( 'NONE', #7204, #15592 ) ;
#2913 = LINE ( 'NONE', #11250, #16427 ) ;
#2914 = ORIENTED_EDGE ( 'NONE', *, *, #12976, .F. ) ;
#2915 = CARTESIAN_POINT ( 'NONE',  ( -71.24615306438080609, 115.9262801152292042, -15.00000000000001421 ) ) ;
#2916 = LINE ( 'NONE', #196, #17336 ) ;
#2917 = ORIENTED_EDGE ( 'NONE', *, *, #17381, .T. ) ;
#2918 = ORIENTED_EDGE ( 'NONE', *, *, #8704, .F. ) ;
#2919 = CARTESIAN_POINT ( 'NONE',  ( -50.06979403241811610, 50.58224449241410525, 57.00000000000000000 ) ) ;
#2920 = DIRECTION ( 'NONE',  ( 0.9396926207859135349, 0.3420201433256547241, -1.086737899652995685E-16 ) ) ;
#2921 = LINE ( 'NONE', #3007, #3548 ) ;
#2922 = DIRECTION ( 'NONE',  ( 0.000000000000000000, 0.000000000000000000, 1.000000000000000000 ) ) ;
#2923 = LINE ( 'NONE', #7221, #1835 ) ;
#2924 = VERTEX_POINT ( 'NONE', #14169 ) ;
#2925 = LINE ( 'NONE', #7398, #11989 ) ;
#2926 = ORIENTED_EDGE ( 'NONE', *, *, #15850, .F. ) ;
#2927 = CARTESIAN_POINT ( 'NONE',  ( -50.41499038512538533, 117.9449492212793444, -2.999999999999999112 ) ) ;
#2928 = CARTESIAN_POINT ( 'NONE',  ( -71.24615306438111872, 18.53690796522925055, 15.00000000000006928 ) ) ;
#2929 = VERTEX_POINT ( 'NONE', #10895 ) ;
#2930 = CARTESIAN_POINT ( 'NONE',  ( -115.3009539377894015, -94.06000857856476216, -6.066633078422342784 ) ) ;
#2931 = ORIENTED_EDGE ( 'NONE', *, *, #4659, .F. ) ;
#2932 = EDGE_CURVE ( 'NONE', #13980, #13829, #15051, .T. ) ;
#2933 = VERTEX_POINT ( 'NONE', #13984 ) ;
#2934 = DIRECTION ( 'NONE',  ( 0.000000000000000000, 1.000000000000000000, 0.000000000000000000 ) ) ;
#2935 = FACE_OUTER_BOUND ( 'NONE', #17821, .T. ) ;
#2936 = PLANE ( 'NONE',  #16182 ) ;
#2937 = ORIENTED_EDGE ( 'NONE', *, *, #9273, .T. ) ;
#2938 = ADVANCED_FACE ( 'NONE', ( #2935 ), #130, .T. ) ;
#2939 = CARTESIAN_POINT ( 'NONE',  ( -25.73217265163131984, -95.23217577251028843, 5.709860606646938841 ) ) ;
#2940 = DIRECTION ( 'NONE',  ( -1.000000000000000000, 2.109423746787799005E-14, 1.387778780781446662E-16 ) ) ;
#2941 = EDGE_LOOP ( 'NONE', ( #12024, #1626, #8222, #4413 ) ) ;
#2942 = AXIS2_PLACEMENT_3D ( 'NONE', #11171, #6954, #18378 ) ;
#2943 = DIRECTION ( 'NONE',  ( 0.000000000000000000, 0.000000000000000000, 1.000000000000000000 ) ) ;
#2944 = DIRECTION ( 'NONE',  ( -1.000000000000000000, 0.000000000000000000, 0.000000000000000000 ) ) ;
#2945 = DIRECTION ( 'NONE',  ( 0.000000000000000000, 1.000000000000000000, 0.000000000000000000 ) ) ;
#2946 = EDGE_LOOP ( 'NONE', ( #1692, #2804, #8014, #17354 ) ) ;
#2947 = DIRECTION ( 'NONE',  ( 1.000000000000000000, 0.000000000000000000, 0.000000000000000000 ) ) ;
#2948 = ORIENTED_EDGE ( 'NONE', *, *, #416, .T. ) ;
#2949 = ORIENTED_EDGE ( 'NONE', *, *, #11587, .T. ) ;
#2950 = CARTESIAN_POINT ( 'NONE',  ( 4.699999999999995737, 7.505553499465141165, -1.387778780781445676E-14 ) ) ;
#2951 = CIRCLE ( 'NONE', #18501, 12.49999999999999645 ) ;
#2952 = ORIENTED_EDGE ( 'NONE', *, *, #18454, .F. ) ;
#2953 = VERTEX_POINT ( 'NONE', #17319 ) ;
#2954 = CARTESIAN_POINT ( 'NONE',  ( -57.08002265617300708, 84.22855780814606419, 28.00000000000000355 ) ) ;
#2955 = DIRECTION ( 'NONE',  ( 0.000000000000000000, 0.000000000000000000, 1.000000000000000000 ) ) ;
#2956 = ORIENTED_EDGE ( 'NONE', *, *, #1640, .T. ) ;
#2957 = DIRECTION ( 'NONE',  ( -5.204170427930409450E-16, 0.000000000000000000, 1.000000000000000000 ) ) ;
#2958 = CARTESIAN_POINT ( 'NONE',  ( -115.7702289486887395, -111.0842361345572158, -5.654315315326000402 ) ) ;
#2959 = CARTESIAN_POINT ( 'NONE',  ( -68.99615306438093398, 42.85071613813026659, 15.00000000000006928 ) ) ;
#2960 = DIRECTION ( 'NONE',  ( 1.156482317317869999E-16, 0.000000000000000000, 1.000000000000000000 ) ) ;
#2961 = ORIENTED_EDGE ( 'NONE', *, *, #14484, .T. ) ;
#2962 = ADVANCED_FACE ( 'NONE', ( #2851 ), #4338, .T. ) ;
#2963 = CARTESIAN_POINT ( 'NONE',  ( -64.18632899337946185, 107.0896764944433954, 102.5000000000000000 ) ) ;
#2964 = VECTOR ( 'NONE', #13241, 1000.000000000000000 ) ;
#2965 = DIRECTION ( 'NONE',  ( 1.000000000000000000, 0.000000000000000000, 0.000000000000000000 ) ) ;
#2966 = CARTESIAN_POINT ( 'NONE',  ( -67.59262256747315689, 117.8748711238780373, 35.00000000000000000 ) ) ;
#2967 = ORIENTED_EDGE ( 'NONE', *, *, #9394, .F. ) ;
#2968 = DIRECTION ( 'NONE',  ( 1.000000000000000000, 2.062304371594500740E-16, 0.000000000000000000 ) ) ;
#2969 = CARTESIAN_POINT ( 'NONE',  ( 93.45071565215914688, 84.22855780814606419, 62.50000000000001421 ) ) ;
#2970 = LINE ( 'NONE', #1477, #6272 ) ;
#2971 = EDGE_LOOP ( 'NONE', ( #13344, #13626, #11676, #4312 ) ) ;
#2972 = EDGE_CURVE ( 'NONE', #4999, #13143, #10222, .T. ) ;
#2973 = ORIENTED_EDGE ( 'NONE', *, *, #3549, .F. ) ;
#2974 = EDGE_CURVE ( 'NONE', #8996, #17731, #3200, .T. ) ;
#2975 = CIRCLE ( 'NONE', #7743, 10.24900000000000766 ) ;
#2976 = DIRECTION ( 'NONE',  ( -1.000000000000000000, -1.632709340522812220E-15, 0.000000000000000000 ) ) ;
#2977 = VECTOR ( 'NONE', #18123, 1000.000000000000000 ) ;
#2978 = DIRECTION ( 'NONE',  ( 1.000000000000000000, 0.000000000000000000, 0.000000000000000000 ) ) ;
#2979 = CARTESIAN_POINT ( 'NONE',  ( -66.34428321731556366, 112.0980243198733177, -27.54384358185309267 ) ) ;
#2980 = DIRECTION ( 'NONE',  ( 0.000000000000000000, 1.000000000000000000, 0.000000000000000000 ) ) ;
#2981 = CARTESIAN_POINT ( 'NONE',  ( -70.06856178257680767, 110.5691553257988460, -22.35917033480641791 ) ) ;
#2982 = ORIENTED_EDGE ( 'NONE', *, *, #6512, .F. ) ;
#2983 = EDGE_CURVE ( 'NONE', #13683, #11287, #11624, .T. ) ;
#2984 = EDGE_CURVE ( 'NONE', #9931, #14963, #7408, .T. ) ;
#2985 = DIRECTION ( 'NONE',  ( 0.3420201433256612189, -0.9396926207859112035, 0.000000000000000000 ) ) ;
#2986 = DIRECTION ( 'NONE',  ( 0.000000000000000000, 1.000000000000000000, 0.000000000000000000 ) ) ;
#2987 = CARTESIAN_POINT ( 'NONE',  ( -39.99251679397033854, 54.40212825384665507, 24.22832327945725339 ) ) ;
#2988 = DIRECTION ( 'NONE',  ( 1.000000000000000000, 0.000000000000000000, 5.077734830647302671E-16 ) ) ;
#2989 = ORIENTED_EDGE ( 'NONE', *, *, #14091, .T. ) ;
#2990 = CARTESIAN_POINT ( 'NONE',  ( -37.13913369598539305, 90.95230598576922887, 65.83182832201505619 ) ) ;
#2991 = DIRECTION ( 'NONE',  ( 1.000000000000000000, 0.000000000000000000, 0.000000000000000000 ) ) ;
#2992 = ORIENTED_EDGE ( 'NONE', *, *, #3112, .F. ) ;
#2993 = ADVANCED_FACE ( 'NONE', ( #4508 ), #10049, .T. ) ;
#2994 = LINE ( 'NONE', #15445, #1790 ) ;
#2995 = VECTOR ( 'NONE', #8546, 1000.000000000000000 ) ;
#2996 = CARTESIAN_POINT ( 'NONE',  ( -68.99615306438094819, 71.12504998813029999, -15.00000000000001421 ) ) ;
#2997 = ORIENTED_EDGE ( 'NONE', *, *, #13144, .T. ) ;
#2998 =( REPRESENTATION_RELATIONSHIP ('NONE','NONE', #359, #5501 ) REPRESENTATION_RELATIONSHIP_WITH_TRANSFORMATION ( #15755 )SHAPE_REPRESENTATION_RELATIONSHIP( ) );
#2999 = EDGE_CURVE ( 'NONE', #5330, #5342, #13049, .T. ) ;
#3000 = VERTEX_POINT ( 'NONE', #15752 ) ;
#3001 = EDGE_CURVE ( 'NONE', #13376, #5348, #8739, .T. ) ;
#3002 = EDGE_CURVE ( 'NONE', #274, #1187, #11776, .T. ) ;
#3003 = ORIENTED_EDGE ( 'NONE', *, *, #13710, .T. ) ;
#3004 = DIRECTION ( 'NONE',  ( 1.000000000000000000, -0.000000000000000000, -0.000000000000000000 ) ) ;
#3005 = FACE_OUTER_BOUND ( 'NONE', #18345, .T. ) ;
#3006 = AXIS2_PLACEMENT_3D ( 'NONE', #7206, #12924, #15632 ) ;
#3007 = CARTESIAN_POINT ( 'NONE',  ( -27.71117476891160081, 84.22855780814606419, 37.50000000000000000 ) ) ;
#3008 = EDGE_CURVE ( 'NONE', #13332, #15988, #296, .T. ) ;
#3009 = CARTESIAN_POINT ( 'NONE',  ( -107.5926225674731853, 60.58224449241411946, -25.00000000000000000 ) ) ;
#3010 = AXIS2_PLACEMENT_3D ( 'NONE', #1602, #16165, #8897 ) ;
#3011 = FACE_OUTER_BOUND ( 'NONE', #4358, .T. ) ;
#3012 = VECTOR ( 'NONE', #460, 1000.000000000000000 ) ;
#3013 = ORIENTED_EDGE ( 'NONE', *, *, #17161, .T. ) ;
#3014 = DIRECTION ( 'NONE',  ( 0.000000000000000000, 0.000000000000000000, 1.000000000000000000 ) ) ;
#3015 = EDGE_LOOP ( 'NONE', ( #1478, #13689, #12574, #8836 ) ) ;
#3016 = DIRECTION ( 'NONE',  ( 0.9396926207859145341, 0.3420201433256520596, 0.000000000000000000 ) ) ;
#3017 = CARTESIAN_POINT ( 'NONE',  ( 103.5381772159376084, -151.5628872026272802, -57.00000000000000000 ) ) ;
#3018 = ORIENTED_EDGE ( 'NONE', *, *, #14027, .T. ) ;
#3019 = CARTESIAN_POINT ( 'NONE',  ( -111.3698580185282054, -91.24992890033504978, -9.348340137070142219 ) ) ;
#3020 = ORIENTED_EDGE ( 'NONE', *, *, #16481, .T. ) ;
#3021 = CIRCLE ( 'NONE', #5401, 29.36884788726140627 ) ;
#3022 = AXIS2_PLACEMENT_3D ( 'NONE', #243, #168, #5933 ) ;
#3023 = ORIENTED_EDGE ( 'NONE', *, *, #9031, .T. ) ;
#3024 = FACE_OUTER_BOUND ( 'NONE', #1420, .T. ) ;
#3025 = DIRECTION ( 'NONE',  ( 0.000000000000000000, -5.551115123125748189E-17, -1.000000000000000000 ) ) ;
#3026 = DIRECTION ( 'NONE',  ( 0.000000000000000000, 0.000000000000000000, 1.000000000000000000 ) ) ;
#3027 = ORIENTED_EDGE ( 'NONE', *, *, #15319, .T. ) ;
#3028 = AXIS2_PLACEMENT_3D ( 'NONE', #10906, #8283, #15184 ) ;
#3029 = EDGE_LOOP ( 'NONE', ( #17481, #3932, #17533, #5533 ) ) ;
#3030 = FACE_OUTER_BOUND ( 'NONE', #3216, .T. ) ;
#3031 = CARTESIAN_POINT ( 'NONE',  ( -57.08002265617300708, 84.22855780814606419, -15.00000000000001421 ) ) ;
#3032 = DIRECTION ( 'NONE',  ( 0.000000000000000000, -1.000000000000000000, 0.000000000000000000 ) ) ;
#3033 = CARTESIAN_POINT ( 'NONE',  ( -76.37409655828219002, -111.0842361345572158, -45.05044770573186952 ) ) ;
#3034 = CIRCLE ( 'NONE', #18273, 5.654315315325682434 ) ;
#3035 = ORIENTED_EDGE ( 'NONE', *, *, #13624, .F. ) ;
#3036 = DIRECTION ( 'NONE',  ( 0.000000000000000000, 1.000000000000000000, 0.000000000000000000 ) ) ;
#3037 = ORIENTED_EDGE ( 'NONE', *, *, #17681, .F. ) ;
#3038 = VERTEX_POINT ( 'NONE', #7333 ) ;
#3039 = VECTOR ( 'NONE', #8549, 1000.000000000000000 ) ;
#3040 = ORIENTED_EDGE ( 'NONE', *, *, #15682, .T. ) ;
#3041 = VECTOR ( 'NONE', #497, 1000.000000000000000 ) ;
#3042 = CIRCLE ( 'NONE', #56, 4.600000000000006750 ) ;
#3043 = DIRECTION ( 'NONE',  ( -0.9396926207859088720, 0.3420201433256675472, -4.890320548438450878E-16 ) ) ;
#3044 = LINE ( 'NONE', #14284, #14457 ) ;
#3045 = ORIENTED_EDGE ( 'NONE', *, *, #6673, .F. ) ;
#3046 = DIRECTION ( 'NONE',  ( 0.000000000000000000, 0.000000000000000000, 1.000000000000000000 ) ) ;
#3047 = DIRECTION ( 'NONE',  ( 1.000000000000000000, 0.000000000000000000, 3.771137991253923150E-16 ) ) ;
#3048 = CYLINDRICAL_SURFACE ( 'NONE', #7497, 4.599999999999992539 ) ;
#3049 = DIRECTION ( 'NONE',  ( -1.000000000000000000, 0.000000000000000000, 0.000000000000000000 ) ) ;
#3050 = VERTEX_POINT ( 'NONE', #1703 ) ;
#3051 = CIRCLE ( 'NONE', #66, 3.999999999999996447 ) ;
#3052 = DIRECTION ( 'NONE',  ( 0.000000000000000000, 0.000000000000000000, 1.000000000000000000 ) ) ;
#3053 = CARTESIAN_POINT ( 'NONE',  ( -48.65098454476478196, 77.46608744949921288, -167.1454815528550739 ) ) ;
#3054 = LINE ( 'NONE', #8946, #2149 ) ;
#3055 = VERTEX_POINT ( 'NONE', #18472 ) ;
#3056 = CIRCLE ( 'NONE', #6627, 3.999999999999982681 ) ;
#3057 = VECTOR ( 'NONE', #7463, 1000.000000000000000 ) ;
#3058 = CARTESIAN_POINT ( 'NONE',  ( -68.99615306438100504, 48.51904558166270220, -167.1454815528550739 ) ) ;
#3059 = CARTESIAN_POINT ( 'NONE',  ( -78.12361985383350316, 84.22855780814606419, 37.50000000000000000 ) ) ;
#3060 = VERTEX_POINT ( 'NONE', #5991 ) ;
#3061 = ORIENTED_EDGE ( 'NONE', *, *, #5283, .F. ) ;
#3062 = VECTOR ( 'NONE', #10050, 1000.000000000000000 ) ;
#3063 = EDGE_CURVE ( 'NONE', #5132, #10265, #10131, .T. ) ;
#3064 = CARTESIAN_POINT ( 'NONE',  ( -68.99615306438094819, 55.41708673813027985, -167.1454815528550739 ) ) ;
#3065 = VECTOR ( 'NONE', #18297, 1000.000000000000000 ) ;
#3066 = AXIS2_PLACEMENT_3D ( 'NONE', #6000, #14705, #1634 ) ;
#3067 =( NAMED_UNIT ( * ) PLANE_ANGLE_UNIT ( ) SI_UNIT ( $, .RADIAN. ) );
#3068 = FACE_OUTER_BOUND ( 'NONE', #7042, .T. ) ;
#3069 = DIRECTION ( 'NONE',  ( -1.000000000000000000, 0.000000000000000000, 0.000000000000000000 ) ) ;
#3070 = DIRECTION ( 'NONE',  ( 0.000000000000000000, 1.000000000000000000, -0.000000000000000000 ) ) ;
#3071 = ORIENTED_EDGE ( 'NONE', *, *, #12937, .F. ) ;
#3072 = CARTESIAN_POINT ( 'NONE',  ( 0.000000000000000000, 0.000000000000000000, 0.000000000000000000 ) ) ;
#3073 = FACE_OUTER_BOUND ( 'NONE', #37, .T. ) ;
#3074 = DIRECTION ( 'NONE',  ( 0.000000000000000000, 0.000000000000000000, 1.000000000000000000 ) ) ;
#3075 = ORIENTED_EDGE ( 'NONE', *, *, #9770, .T. ) ;
#3076 = ADVANCED_FACE ( 'NONE', ( #9957 ), #11719, .T. ) ;
#3077 = CARTESIAN_POINT ( 'NONE',  ( -37.02218768164058815, 90.59536451873519525, 66.47148242010926822 ) ) ;
#3078 = AXIS2_PLACEMENT_3D ( 'NONE', #6362, #9279, #12180 ) ;
#3079 = EDGE_CURVE ( 'NONE', #11670, #17138, #17736, .T. ) ;
#3080 = DIRECTION ( 'NONE',  ( 1.000000000000000000, 0.000000000000000000, 5.551115123125786646E-16 ) ) ;
#3081 = ORIENTED_EDGE ( 'NONE', *, *, #331, .T. ) ;
#3082 = VECTOR ( 'NONE', #15623, 1000.000000000000000 ) ;
#3083 = CARTESIAN_POINT ( 'NONE',  ( -71.24615306438103346, 40.52805651522925245, 15.00000000000006928 ) ) ;
#3084 = VECTOR ( 'NONE', #4411, 1000.000000000000000 ) ;
#3085 = CARTESIAN_POINT ( 'NONE',  ( -53.44817431141344599, 74.64462966772957486, -15.00000000000001421 ) ) ;
#3086 = VERTEX_POINT ( 'NONE', #14607 ) ;
#3087 = VECTOR ( 'NONE', #256, 1000.000000000000000 ) ;
#3088 = VERTEX_POINT ( 'NONE', #1792 ) ;
#3089 = EDGE_CURVE ( 'NONE', #8537, #16154, #12776, .T. ) ;
#3090 = EDGE_CURVE ( 'NONE', #15763, #4483, #15666, .T. ) ;
#3091 = EDGE_CURVE ( 'NONE', #16133, #15911, #2160, .T. ) ;
#3092 = ORIENTED_EDGE ( 'NONE', *, *, #18301, .T. ) ;
#3093 = CARTESIAN_POINT ( 'NONE',  ( -97.59262256747319952, 57.88796029049330372, -22.35917033480642502 ) ) ;
#3094 = LINE ( 'NONE', #13197, #3680 ) ;
#3095 = DIRECTION ( 'NONE',  ( -1.000000000000000000, 0.000000000000000000, 0.000000000000000000 ) ) ;
#3096 = CARTESIAN_POINT ( 'NONE',  ( -68.99615306438111872, 13.96152643166267993, -15.00000000000001421 ) ) ;
#3097 = EDGE_CURVE ( 'NONE', #3566, #3387, #8198, .T. ) ;
#3098 = VECTOR ( 'NONE', #12885, 1000.000000000000000 ) ;
#3099 = VECTOR ( 'NONE', #10921, 1000.000000000000000 ) ;
#3100 = FACE_OUTER_BOUND ( 'NONE', #11232, .T. ) ;
#3101 = ORIENTED_EDGE ( 'NONE', *, *, #11657, .T. ) ;
#3102 = ADVANCED_FACE ( 'NONE', ( #17507, #7500 ), #3375, .F. ) ;
#3103 = EDGE_CURVE ( 'NONE', #1000, #16773, #9006, .T. ) ;
#3104 = FACE_OUTER_BOUND ( 'NONE', #8926, .T. ) ;
#3105 = DIRECTION ( 'NONE',  ( -0.000000000000000000, -0.000000000000000000, 1.000000000000000000 ) ) ;
#3106 = EDGE_CURVE ( 'NONE', #4868, #11956, #4685, .T. ) ;
#3107 = CARTESIAN_POINT ( 'NONE',  ( -68.99615306438089135, 83.07656473166271383, 15.00000000000006928 ) ) ;
#3108 = ORIENTED_EDGE ( 'NONE', *, *, #16825, .T. ) ;
#3109 = DIRECTION ( 'NONE',  ( 0.3420201433256686574, -0.9396926207859084279, 0.000000000000000000 ) ) ;
#3110 = DIRECTION ( 'NONE',  ( 1.000000000000000000, 1.890137176791858990E-15, 0.000000000000000000 ) ) ;
#3111 = VERTEX_POINT ( 'NONE', #9190 ) ;
#3112 = EDGE_CURVE ( 'NONE', #4238, #15911, #11986, .T. ) ;
#3113 = ORIENTED_EDGE ( 'NONE', *, *, #1188, .F. ) ;
#3114 = ADVANCED_FACE ( 'NONE', ( #2071 ), #17585, .F. ) ;
#3115 = AXIS2_PLACEMENT_3D ( 'NONE', #16141, #445, #6315 ) ;
#3116 = ADVANCED_FACE ( 'NONE', ( #7870 ), #1985, .T. ) ;
#3117 = AXIS2_PLACEMENT_3D ( 'NONE', #11158, #11055, #13674 ) ;
#3118 = VERTEX_POINT ( 'NONE', #3560 ) ;
#3119 = DIRECTION ( 'NONE',  ( -0.000000000000000000, -0.000000000000000000, -1.000000000000000000 ) ) ;
#3120 = CARTESIAN_POINT ( 'NONE',  ( -68.99615306438117557, 4.536748481662661092, -167.1454815528550739 ) ) ;
#3121 = LINE ( 'NONE', #14347, #3062 ) ;
#3122 = AXIS2_PLACEMENT_3D ( 'NONE', #7521, #10240, #8854 ) ;
#3123 = ORIENTED_EDGE ( 'NONE', *, *, #242, .T. ) ;
#3124 = CARTESIAN_POINT ( 'NONE',  ( -25.66933353722515676, -96.08423613455721579, 5.654315315325685987 ) ) ;
#3125 = EDGE_LOOP ( 'NONE', ( #53, #5669, #3865, #17124, #6168, #17356, #13435, #10412, #14241, #477, #15134, #9001, #3749, #17717, #15653, #1934, #9819, #6511, #8617, #1701, #5467, #493, #13429, #2220, #5267, #6264, #4443, #1265, #18015, #5748, #12975, #9004, #4502, #14300, #13408, #17515, #15615, #9986, #12555, #7195, #8751, #10596, #1400, #14999, #6564, #4438, #12956, #15571, #17226, #9617, #15147, #7025, #13213, #1311, #11706, #17809, #13812, #781, #13997, #17054, #15429, #1586, #12151, #10761, #4672, #13203, #17, #8565, #9427, #6617, #10419, #14798, #2741, #18206, #10732, #13861, #14836, #18360, #17168, #519, #7980, #17026, #11221, #6130, #17141, #5619, #8711, #1993, #16461, #11597, #6014, #5345, #16094, #12015, #11041 ) ) ;
#3126 = VECTOR ( 'NONE', #4581, 1000.000000000000000 ) ;
#3127 = DIRECTION ( 'NONE',  ( 0.000000000000000000, 0.000000000000000000, 1.000000000000000000 ) ) ;
#3128 = DIRECTION ( 'NONE',  ( 1.156482317317869999E-16, 0.000000000000000000, 1.000000000000000000 ) ) ;
#3129 = CARTESIAN_POINT ( 'NONE',  ( -92.59262256747321373, 110.5691553257988460, 22.35917033480641791 ) ) ;
#3130 = LINE ( 'NONE', #15760, #9344 ) ;
#3131 = AXIS2_PLACEMENT_3D ( 'NONE', #6194, #17615, #1651 ) ;
#3132 = ORIENTED_EDGE ( 'NONE', *, *, #9786, .F. ) ;
#3133 = EDGE_CURVE ( 'NONE', #7544, #881, #1892, .T. ) ;
#3134 = AXIS2_PLACEMENT_3D ( 'NONE', #4485, #3004, #15904 ) ;
#3135 = EDGE_CURVE ( 'NONE', #5784, #12176, #10400, .T. ) ;
#3136 = CARTESIAN_POINT ( 'NONE',  ( -57.08002265617300708, 84.22855780814606419, 37.50000000000000000 ) ) ;
#3137 = ORIENTED_EDGE ( 'NONE', *, *, #15912, .T. ) ;
#3138 = EDGE_LOOP ( 'NONE', ( #7995, #4313, #2910, #273 ) ) ;
#3139 = VECTOR ( 'NONE', #15929, 1000.000000000000000 ) ;
#3140 = ORIENTED_EDGE ( 'NONE', *, *, #5509, .T. ) ;
#3141 = VECTOR ( 'NONE', #10571, 1000.000000000000114 ) ;
#3142 = VECTOR ( 'NONE', #12538, 1000.000000000000000 ) ;
#3143 = FACE_OUTER_BOUND ( 'NONE', #16817, .T. ) ;
#3144 = CARTESIAN_POINT ( 'NONE',  ( -42.53669312409158465, -91.08423613455721579, -10.65431531532567533 ) ) ;
#3145 = ORIENTED_EDGE ( 'NONE', *, *, #1525, .T. ) ;
#3146 = DIRECTION ( 'NONE',  ( 0.000000000000000000, 0.000000000000000000, 1.000000000000000000 ) ) ;
#3147 = LINE ( 'NONE', #4367, #10144 ) ;
#3148 = LINE ( 'NONE', #15860, #12291 ) ;
#3149 = DIRECTION ( 'NONE',  ( -5.204170427930409450E-16, 0.000000000000000000, 1.000000000000000000 ) ) ;
#3150 = VERTEX_POINT ( 'NONE', #4873 ) ;
#3151 = DIRECTION ( 'NONE',  ( 0.000000000000000000, 0.000000000000000000, 1.000000000000000000 ) ) ;
#3152 = CARTESIAN_POINT ( 'NONE',  ( -44.78895386838529902, 81.95267818613812949, -15.00000000000001421 ) ) ;
#3153 = DIRECTION ( 'NONE',  ( -1.000000000000000000, 0.000000000000000000, 0.000000000000000000 ) ) ;
#3154 = ORIENTED_EDGE ( 'NONE', *, *, #11457, .T. ) ;
#3155 = CIRCLE ( 'NONE', #8835, 42.49926016644912607 ) ;
#3156 = COLOUR_RGB ( '',0.7921568627450980005, 0.8196078431372548767, 0.9333333333333333481 ) ;
#3157 = AXIS2_PLACEMENT_3D ( 'NONE', #3719, #2604, #3611 ) ;
#3158 = LINE ( 'NONE', #5771, #7043 ) ;
#3159 = FACE_OUTER_BOUND ( 'NONE', #17830, .T. ) ;
#3160 = ORIENTED_EDGE ( 'NONE', *, *, #3423, .T. ) ;
#3161 = ORIENTED_EDGE ( 'NONE', *, *, #9186, .F. ) ;
#3162 = ORIENTED_EDGE ( 'NONE', *, *, #3781, .T. ) ;
#3164 = EDGE_CURVE ( 'NONE', #60, #3192, #9096, .T. ) ;
#3163 = DIRECTION ( 'NONE',  ( 0.000000000000000000, 1.245108978942215720E-14, 1.000000000000000000 ) ) ;
#3165 = CARTESIAN_POINT ( 'NONE',  ( -66.27751174112272281, 84.22855780814606419, 77.50000000000000000 ) ) ;
#3166 = CARTESIAN_POINT ( 'NONE',  ( -68.99615306438094819, 64.22700883166265839, 15.00000000000006928 ) ) ;
#3167 = VERTEX_POINT ( 'NONE', #6171 ) ;
#3168 = DIRECTION ( 'NONE',  ( -1.000000000000000000, -2.062304371594500247E-16, -0.000000000000000000 ) ) ;
#3169 = LINE ( 'NONE', #12049, #10628 ) ;
#3170 = CARTESIAN_POINT ( 'NONE',  ( 5.299999999999998934, 0.000000000000000000, 0.000000000000000000 ) ) ;
#3171 = DIRECTION ( 'NONE',  ( 0.3420201433256649937, 0.9396926207859097602, -0.000000000000000000 ) ) ;
#3172 = CARTESIAN_POINT ( 'NONE',  ( -37.06251219239532446, 90.72064142110004070, 58.73664414705599768 ) ) ;
#3173 = PLANE ( 'NONE',  #17051 ) ;
#3174 = ORIENTED_EDGE ( 'NONE', *, *, #17928, .T. ) ;
#3175 = CARTESIAN_POINT ( 'NONE',  ( -66.09688823571623573, 58.56582669723388790, 25.00000000000000711 ) ) ;
#3176 = DIRECTION ( 'NONE',  ( -1.000000000000000000, 0.000000000000000000, 1.692578276882434470E-16 ) ) ;
#3177 = ORIENTED_EDGE ( 'NONE', *, *, #6287, .T. ) ;
#3178 = ORIENTED_EDGE ( 'NONE', *, *, #4773, .F. ) ;
#3180 = ADVANCED_FACE ( 'NONE', ( #12179 ), #14968, .T. ) ;
#3179 = VERTEX_POINT ( 'NONE', #12090 ) ;
#3181 = DIRECTION ( 'NONE',  ( -1.000000000000000000, 0.000000000000000000, 1.692578276882436442E-16 ) ) ;
#3182 = DIRECTION ( 'NONE',  ( -0.000000000000000000, -0.000000000000000000, -1.000000000000000000 ) ) ;
#3183 = CARTESIAN_POINT ( 'NONE',  ( -77.66397652102858729, 79.84943054288078201, 68.59368636907963435 ) ) ;
#3184 = DIRECTION ( 'NONE',  ( 1.000000000000000000, 0.000000000000000000, 0.000000000000000000 ) ) ;
#3185 = DIRECTION ( 'NONE',  ( -1.000000000000000000, -0.000000000000000000, -0.000000000000000000 ) ) ;
#3186 = LINE ( 'NONE', #281, #12301 ) ;
#3187 = VERTEX_POINT ( 'NONE', #17784 ) ;
#3188 = DIRECTION ( 'NONE',  ( 1.000000000000000000, 0.000000000000000000, 5.204170427930409450E-16 ) ) ;
#3189 = EDGE_CURVE ( 'NONE', #4169, #1925, #6402, .T. ) ;
#3190 = CARTESIAN_POINT ( 'NONE',  ( -70.71978124295696944, -111.0842361345572158, 5.204170427930421283E-15 ) ) ;
#3191 = CARTESIAN_POINT ( 'NONE',  ( -68.99615306438117557, 1.395155831662693524, -15.00000000000001421 ) ) ;
#3192 = VERTEX_POINT ( 'NONE', #3656 ) ;
#3193 = DIRECTION ( 'NONE',  ( 0.000000000000000000, 0.000000000000000000, 1.000000000000000000 ) ) ;
#3194 = DIRECTION ( 'NONE',  ( 1.000000000000000000, 0.000000000000000000, 0.000000000000000000 ) ) ;
#3195 = EDGE_LOOP ( 'NONE', ( #17452, #9590, #17464, #18351 ) ) ;
#3196 = EDGE_CURVE ( 'NONE', #2889, #11833, #4600, .T. ) ;
#3197 = VERTEX_POINT ( 'NONE', #8254 ) ;
#3198 = EDGE_CURVE ( 'NONE', #16032, #15619, #18260, .T. ) ;
#3199 = LINE ( 'NONE', #17234, #3139 ) ;
#3200 = LINE ( 'NONE', #13125, #5506 ) ;
#3201 = CARTESIAN_POINT ( 'NONE',  ( -68.99615306438086293, 92.50134268166266338, -15.00000000000001421 ) ) ;
#3202 = ORIENTED_EDGE ( 'NONE', *, *, #1512, .T. ) ;
#3203 = VERTEX_POINT ( 'NONE', #12666 ) ;
#3204 = EDGE_CURVE ( 'NONE', #14281, #13941, #9549, .T. ) ;
#3205 = LINE ( 'NONE', #10406, #11096 ) ;
#3206 = DIRECTION ( 'NONE',  ( 0.000000000000000000, 1.000000000000000000, 0.000000000000000000 ) ) ;
#3207 = CARTESIAN_POINT ( 'NONE',  ( -71.24615306438080609, 115.9262801152292042, -167.1454815528550739 ) ) ;
#3208 = EDGE_CURVE ( 'NONE', #8420, #9318, #18050, .T. ) ;
#3209 = CARTESIAN_POINT ( 'NONE',  ( -57.08002265617300708, 84.22855780814606419, 37.50000000000000000 ) ) ;
#3210 = ADVANCED_FACE ( 'NONE', ( #10965 ), #15455, .F. ) ;
#3211 = VERTEX_POINT ( 'NONE', #956 ) ;
#3212 = CARTESIAN_POINT ( 'NONE',  ( -92.59262256747319952, 57.88796029049330372, -26.35917033480641436 ) ) ;
#3213 = VERTEX_POINT ( 'NONE', #9651 ) ;
#3214 = EDGE_CURVE ( 'NONE', #15197, #15151, #12698, .T. ) ;
#3215 = DIRECTION ( 'NONE',  ( 1.000000000000000000, 0.000000000000000000, 0.000000000000000000 ) ) ;
#3216 = EDGE_LOOP ( 'NONE', ( #8491, #17094, #10489, #14441 ) ) ;
#3217 = ADVANCED_FACE ( 'NONE', ( #6754 ), #1061, .T. ) ;
#3218 = ORIENTED_EDGE ( 'NONE', *, *, #6166, .T. ) ;
#3219 = EDGE_CURVE ( 'NONE', #15837, #17074, #7017, .T. ) ;
#3220 = LINE ( 'NONE', #10421, #10009 ) ;
#3221 = EDGE_CURVE ( 'NONE', #13519, #4088, #2513, .T. ) ;
#3222 = DIRECTION ( 'NONE',  ( 1.000000000000000000, 0.000000000000000000, 0.000000000000000000 ) ) ;
#3223 = EDGE_LOOP ( 'NONE', ( #15642, #13398, #13303, #18519 ) ) ;
#3224 = DIRECTION ( 'NONE',  ( 2.775557561562891351E-16, 0.000000000000000000, 1.000000000000000000 ) ) ;
#3225 = LINE ( 'NONE', #1650, #17649 ) ;
#3226 = CARTESIAN_POINT ( 'NONE',  ( 0.05458999538772711657, -1.264741368073410532, 6.499999999999984013 ) ) ;
#3227 = VERTEX_POINT ( 'NONE', #5538 ) ;
#3228 = ADVANCED_FACE ( 'NONE', ( #6839 ), #18073, .T. ) ;
#3229 = PLANE ( 'NONE',  #3022 ) ;
#3230 = CARTESIAN_POINT ( 'NONE',  ( -71.24615306438114715, 12.25372266522925457, -167.1454815528550739 ) ) ;
#3231 = DIRECTION ( 'NONE',  ( 1.000000000000000000, 0.000000000000000000, 0.000000000000000000 ) ) ;
#3232 = ORIENTED_EDGE ( 'NONE', *, *, #6624, .T. ) ;
#3233 = CARTESIAN_POINT ( 'NONE',  ( -71.24615306438094819, 68.80239036522922902, -15.00000000000001421 ) ) ;
#3234 = VECTOR ( 'NONE', #9115, 1000.000000000000000 ) ;
#3235 = CARTESIAN_POINT ( 'NONE',  ( -71.24615306438076345, 132.5231141045637457, -167.1454815528550739 ) ) ;
#3236 = VERTEX_POINT ( 'NONE', #12471 ) ;
#3237 = ORIENTED_EDGE ( 'NONE', *, *, #6537, .T. ) ;
#3238 = ORIENTED_EDGE ( 'NONE', *, *, #7535, .T. ) ;
#3239 = DIRECTION ( 'NONE',  ( -1.000000000000000000, 0.000000000000000000, -0.000000000000000000 ) ) ;
#3240 = CARTESIAN_POINT ( 'NONE',  ( 0.000000000000000000, 0.000000000000000000, 0.000000000000000000 ) ) ;
#3241 = DIRECTION ( 'NONE',  ( 0.000000000000000000, 0.000000000000000000, 1.000000000000000000 ) ) ;
#3242 = DIRECTION ( 'NONE',  ( 0.000000000000000000, 0.000000000000000000, -1.000000000000000000 ) ) ;
#3243 = AXIS2_PLACEMENT_3D ( 'NONE', #10958, #9363, #16732 ) ;
#3244 = CARTESIAN_POINT ( 'NONE',  ( -71.24615306438089135, 85.39922435456371375, -167.1454815528550739 ) ) ;
#3245 = VERTEX_POINT ( 'NONE', #14052 ) ;
#3246 = DIRECTION ( 'NONE',  ( 0.000000000000000000, 5.551115123125747573E-17, 1.000000000000000000 ) ) ;
#3247 = PLANE ( 'NONE',  #7636 ) ;
#3248 = CARTESIAN_POINT ( 'NONE',  ( -57.56709772515574031, 94.46597735006069740, 15.00000000000006928 ) ) ;
#3249 = DIRECTION ( 'NONE',  ( 0.9396926207859084279, 0.3420201433256686574, 0.000000000000000000 ) ) ;
#3250 = DIRECTION ( 'NONE',  ( 1.000000000000000000, 0.000000000000000000, 3.771137991253928573E-16 ) ) ;
#3251 = DIRECTION ( 'NONE',  ( 0.000000000000000000, 1.000000000000000000, 0.000000000000000000 ) ) ;
#3252 = EDGE_LOOP ( 'NONE', ( #210, #4323, #1274, #11764 ) ) ;
#3253 = CARTESIAN_POINT ( 'NONE',  ( -67.25653033657522428, 61.05141432888216713, 25.00000000000000355 ) ) ;
#3254 = CARTESIAN_POINT ( 'NONE',  ( -36.05420706246012230, 83.23774243329727085, 55.04948847454055283 ) ) ;
#3255 = ORIENTED_EDGE ( 'NONE', *, *, #15679, .T. ) ;
#3256 = VECTOR ( 'NONE', #10033, 1000.000000000000000 ) ;
#3257 = ORIENTED_EDGE ( 'NONE', *, *, #4797, .F. ) ;
#3258 = ADVANCED_FACE ( 'NONE', ( #2258 ), #3709, .F. ) ;
#3259 = VECTOR ( 'NONE', #14561, 999.9999999999998863 ) ;
#3260 = EDGE_LOOP ( 'NONE', ( #5457, #11693, #5313, #13019 ) ) ;
#3261 = CARTESIAN_POINT ( 'NONE',  ( -68.99615306438091977, 73.65178678166269322, 15.00000000000006928 ) ) ;
#3262 = LINE ( 'NONE', #11872, #15926 ) ;
#3263 = CARTESIAN_POINT ( 'NONE',  ( -68.99615306438076345, 96.25779118813024127, 15.00000000000006928 ) ) ;
#3264 = CARTESIAN_POINT ( 'NONE',  ( -94.45685920050698314, -2.213358015103445098, -15.00000000000001421 ) ) ;
#3265 = CARTESIAN_POINT ( 'NONE',  ( 0.000000000000000000, 0.000000000000000000, 0.000000000000000000 ) ) ;
#3266 = CARTESIAN_POINT ( 'NONE',  ( -57.08002265617300708, 84.22855780814606419, -167.1454815528550739 ) ) ;
#3267 = DIRECTION ( 'NONE',  ( -0.000000000000000000, -1.000000000000000000, -0.000000000000000000 ) ) ;
#3268 = ORIENTED_EDGE ( 'NONE', *, *, #232, .T. ) ;
#3269 = CIRCLE ( 'NONE', #8654, 12.50000000000001066 ) ;
#3270 = DIRECTION ( 'NONE',  ( 1.000000000000000000, 0.000000000000000000, 0.000000000000000000 ) ) ;
#3271 = CARTESIAN_POINT ( 'NONE',  ( -53.44817431141344599, 74.64462966772957486, 15.00000000000006928 ) ) ;
#3272 = AXIS2_PLACEMENT_3D ( 'NONE', #6462, #3661, #9373 ) ;
#3273 = DIRECTION ( 'NONE',  ( 0.000000000000000000, 1.000000000000000000, 0.000000000000000000 ) ) ;
#3274 = VERTEX_POINT ( 'NONE', #5334 ) ;
#3275 = CARTESIAN_POINT ( 'NONE',  ( 105.4583593777968105, 56.41207303426870112, -7.000000000000010658 ) ) ;
#3276 = DIRECTION ( 'NONE',  ( -1.000000000000000000, 3.016910393003138520E-15, 0.000000000000000000 ) ) ;
#3277 = ORIENTED_EDGE ( 'NONE', *, *, #9487, .F. ) ;
#3278 = AXIS2_PLACEMENT_3D ( 'NONE', #15467, #10976, #2458 ) ;
#3279 = ORIENTED_EDGE ( 'NONE', *, *, #5010, .F. ) ;
#3280 = EDGE_CURVE ( 'NONE', #5742, #12056, #8153, .T. ) ;
#3281 = CIRCLE ( 'NONE', #7774, 7.168074330098680669 ) ;
#3282 = DIRECTION ( 'NONE',  ( 0.000000000000000000, 0.000000000000000000, -1.000000000000000000 ) ) ;
#3283 = CARTESIAN_POINT ( 'NONE',  ( -68.99615306438082030, 83.69142058813027063, 15.00000000000006928 ) ) ;
#3284 = LINE ( 'NONE', #17586, #4839 ) ;
#3285 = ORIENTED_EDGE ( 'NONE', *, *, #16606, .T. ) ;
#3286 = ORIENTED_EDGE ( 'NONE', *, *, #12003, .T. ) ;
#3287 = DIRECTION ( 'NONE',  ( 1.000000000000000000, 2.062304371594500494E-16, -0.000000000000000000 ) ) ;
#3288 = CARTESIAN_POINT ( 'NONE',  ( -71.24615306438067819, 144.2006139652292518, 15.00000000000006928 ) ) ;
#3289 = CARTESIAN_POINT ( 'NONE',  ( -57.08002265617300708, 84.22855780814606419, -47.50000000000000000 ) ) ;
#3290 = CARTESIAN_POINT ( 'NONE',  ( -71.24615306438070661, 135.6647067545637242, -15.00000000000001421 ) ) ;
#3291 = ORIENTED_EDGE ( 'NONE', *, *, #6289, .T. ) ;
#3293 = ADVANCED_FACE ( 'NONE', ( #6940 ), #5251, .T. ) ;
#3292 = VECTOR ( 'NONE', #14577, 1000.000000000000000 ) ;
#3294 = FACE_OUTER_BOUND ( 'NONE', #11784, .T. ) ;
#3295 = ORIENTED_EDGE ( 'NONE', *, *, #1425, .T. ) ;
#3296 = DIRECTION ( 'NONE',  ( 0.000000000000000000, 0.000000000000000000, -1.000000000000000000 ) ) ;
#3297 = EDGE_LOOP ( 'NONE', ( #12103, #7207, #13916, #8729 ) ) ;
#3298 = ORIENTED_EDGE ( 'NONE', *, *, #15306, .T. ) ;
#3299 = VERTEX_POINT ( 'NONE', #18163 ) ;
#3300 = EDGE_CURVE ( 'NONE', #10126, #7359, #8795, .T. ) ;
#3301 = CIRCLE ( 'NONE', #3609, 9.999999999999994671 ) ;
#3302 = EDGE_CURVE ( 'NONE', #1161, #12615, #854, .T. ) ;
#3303 = CYLINDRICAL_SURFACE ( 'NONE', #1002, 10.24900000000000055 ) ;
#3304 = ORIENTED_EDGE ( 'NONE', *, *, #13286, .T. ) ;
#3305 = AXIS2_PLACEMENT_3D ( 'NONE', #2100, #7809, #9127 ) ;
#3306 = CARTESIAN_POINT ( 'NONE',  ( -57.08002265617300708, 84.22855780814606419, 15.00000000000006928 ) ) ;
#3307 = FACE_OUTER_BOUND ( 'NONE', #7939, .T. ) ;
#3308 = CARTESIAN_POINT ( 'NONE',  ( -71.24615306438070661, 147.3422066152292871, -15.00000000000001421 ) ) ;
#3309 = VERTEX_POINT ( 'NONE', #10868 ) ;
#3310 = EDGE_CURVE ( 'NONE', #15460, #7762, #15952, .T. ) ;
#3311 = PLANE ( 'NONE',  #5987 ) ;
#3312 = EDGE_CURVE ( 'NONE', #3784, #10391, #11535, .T. ) ;
#3313 = PLANE ( 'NONE',  #1558 ) ;
#3314 = DIRECTION ( 'NONE',  ( -5.204170427930409450E-16, 0.000000000000000000, 1.000000000000000000 ) ) ;
#3315 = ORIENTED_EDGE ( 'NONE', *, *, #10863, .T. ) ;
#3316 = CIRCLE ( 'NONE', #10806, 12.50000000000000355 ) ;
#3317 = EDGE_CURVE ( 'NONE', #16328, #8559, #14330, .T. ) ;
#3318 = LINE ( 'NONE', #12129, #17174 ) ;
#3319 = EDGE_CURVE ( 'NONE', #8820, #2089, #4320, .T. ) ;
#3320 = LINE ( 'NONE', #11660, #14370 ) ;
#3321 = VECTOR ( 'NONE', #1797, 1000.000000000000000 ) ;
#3322 = VECTOR ( 'NONE', #381, 1000.000000000000000 ) ;
#3323 = EDGE_LOOP ( 'NONE', ( #15480, #10089, #14610, #12467 ) ) ;
#3324 = ORIENTED_EDGE ( 'NONE', *, *, #5025, .T. ) ;
#3325 = EDGE_CURVE ( 'NONE', #15057, #5292, #15540, .T. ) ;
#3326 = ORIENTED_EDGE ( 'NONE', *, *, #5172, .T. ) ;
#3327 = DIRECTION ( 'NONE',  ( 1.000000000000000000, 2.062304371594500494E-16, 0.000000000000000000 ) ) ;
#3328 = CIRCLE ( 'NONE', #17970, 10.24900000000001477 ) ;
#3329 = LINE ( 'NONE', #12139, #9120 ) ;
#3330 = LINE ( 'NONE', #348, #13531 ) ;
#3331 = CARTESIAN_POINT ( 'NONE',  ( -92.59262256747319952, 57.88796029049329661, -30.35917033480640370 ) ) ;
#3332 = VERTEX_POINT ( 'NONE', #11342 ) ;
#3333 = CARTESIAN_POINT ( 'NONE',  ( -71.24615306438086293, 100.2183168652291982, -15.00000000000001421 ) ) ;
#3334 = VECTOR ( 'NONE', #10433, 1000.000000000000000 ) ;
#3335 = AXIS2_PLACEMENT_3D ( 'NONE', #3437, #3338, #9153 ) ;
#3336 = CARTESIAN_POINT ( 'NONE',  ( -83.23321842955245131, 73.26749283226919829, 102.5000000000000000 ) ) ;
#3337 = DIRECTION ( 'NONE',  ( -1.000000000000000000, -1.332267629550188795E-14, 1.387778780781446662E-16 ) ) ;
#3338 = DIRECTION ( 'NONE',  ( -1.000000000000000000, -0.000000000000000000, -0.000000000000000000 ) ) ;
#3339 = CARTESIAN_POINT ( 'NONE',  ( -36.29790135706344500, 87.56725157785861313, 55.76609545620163999 ) ) ;
#3340 = ORIENTED_EDGE ( 'NONE', *, *, #6518, .T. ) ;
#3341 = CARTESIAN_POINT ( 'NONE',  ( -42.53669312409158465, -96.08423613455721579, -5.654315315325675328 ) ) ;
#3342 = ADVANCED_FACE ( 'NONE', ( #8 ), #15739, .T. ) ;
#3343 = ORIENTED_EDGE ( 'NONE', *, *, #15306, .F. ) ;
#3344 = VECTOR ( 'NONE', #12777, 1000.000000000000000 ) ;
#3345 = LINE ( 'NONE', #13279, #15243 ) ;
#3346 = DIRECTION ( 'NONE',  ( 0.000000000000000000, 0.000000000000000000, 1.000000000000000000 ) ) ;
#3347 = ORIENTED_EDGE ( 'NONE', *, *, #123, .F. ) ;
#3348 = ORIENTED_EDGE ( 'NONE', *, *, #7773, .T. ) ;
#3349 = AXIS2_PLACEMENT_3D ( 'NONE', #14966, #10866, #10591 ) ;
#3350 = VECTOR ( 'NONE', #16574, 1000.000000000000000 ) ;
#3351 = ORIENTED_EDGE ( 'NONE', *, *, #3221, .T. ) ;
#3352 = DIRECTION ( 'NONE',  ( 0.000000000000000000, -1.000000000000000000, 0.000000000000000000 ) ) ;
#3353 = LINE ( 'NONE', #4952, #2482 ) ;
#3354 = DIRECTION ( 'NONE',  ( 0.000000000000000000, 0.000000000000000000, -1.000000000000000000 ) ) ;
#3355 = AXIS2_PLACEMENT_3D ( 'NONE', #2342, #1938, #7645 ) ;
#3356 = CYLINDRICAL_SURFACE ( 'NONE', #14932, 9.999999999999994671 ) ;
#3357 = DIRECTION ( 'NONE',  ( -1.000000000000000000, 0.000000000000000000, 0.000000000000000000 ) ) ;
#3358 = FACE_OUTER_BOUND ( 'NONE', #13694, .T. ) ;
#3359 = ORIENTED_EDGE ( 'NONE', *, *, #5390, .F. ) ;
#3360 = FACE_OUTER_BOUND ( 'NONE', #10097, .T. ) ;
#3361 = CARTESIAN_POINT ( 'NONE',  ( -68.12361985383350316, 84.22855780814606419, -124.8487082408420861 ) ) ;
#3362 = AXIS2_PLACEMENT_3D ( 'NONE', #1060, #6752, #1424 ) ;
#3363 = AXIS2_PLACEMENT_3D ( 'NONE', #4496, #7399, #3016 ) ;
#3364 = AXIS2_PLACEMENT_3D ( 'NONE', #4721, #13171, #14565 ) ;
#3365 = PLANE ( 'NONE',  #1510 ) ;
#3366 = EDGE_LOOP ( 'NONE', ( #8412, #7266 ) ) ;
#3367 = CARTESIAN_POINT ( 'NONE',  ( -57.08002265617300708, 84.22855780814606419, -15.00000000000001421 ) ) ;
#3368 = DIRECTION ( 'NONE',  ( -1.000000000000000000, 0.000000000000000000, 0.000000000000000000 ) ) ;
#3369 = ORIENTED_EDGE ( 'NONE', *, *, #10127, .T. ) ;
#3370 = VECTOR ( 'NONE', #814, 1000.000000000000114 ) ;
#3371 = VERTEX_POINT ( 'NONE', #278 ) ;
#3372 = AXIS2_PLACEMENT_3D ( 'NONE', #8660, #1551, #7259 ) ;
#3373 = AXIS2_PLACEMENT_3D ( 'NONE', #5947, #13260, #14388 ) ;
#3374 = LINE ( 'NONE', #14791, #18483 ) ;
#3375 = PLANE ( 'NONE',  #14467 ) ;
#3376 = EDGE_CURVE ( 'NONE', #9602, #3839, #4404, .T. ) ;
#3377 = LINE ( 'NONE', #10401, #4561 ) ;
#3378 = ORIENTED_EDGE ( 'NONE', *, *, #6649, .F. ) ;
#3379 = CARTESIAN_POINT ( 'NONE',  ( -71.24615306438117557, 6.859408104563785358, 15.00000000000006928 ) ) ;
#3380 = ORIENTED_EDGE ( 'NONE', *, *, #2984, .F. ) ;
#3381 = FACE_OUTER_BOUND ( 'NONE', #528, .T. ) ;
#3382 = CARTESIAN_POINT ( 'NONE',  ( -63.91856434051376823, 76.59466308582156557, 15.00000000000006928 ) ) ;
#3383 = CARTESIAN_POINT ( 'NONE',  ( -77.02091161636059269, 90.95230598576924308, 59.16817167798495802 ) ) ;
#3384 = CARTESIAN_POINT ( 'NONE',  ( -115.3009539377894868, -94.06000857856477637, 6.066633078421709513 ) ) ;
#3385 = ORIENTED_EDGE ( 'NONE', *, *, #1707, .F. ) ;
#3386 = DIRECTION ( 'NONE',  ( 0.000000000000000000, 0.000000000000000000, -1.000000000000000000 ) ) ;
#3387 = VERTEX_POINT ( 'NONE', #11437 ) ;
#3388 = AXIS2_PLACEMENT_3D ( 'NONE', #10448, #17744, #4554 ) ;
#3389 = LINE ( 'NONE', #588, #4146 ) ;
#3391 = ORIENTED_EDGE ( 'NONE', *, *, #9855, .T. ) ;
#3390 = AXIS2_PLACEMENT_3D ( 'NONE', #6309, #522, #9501 ) ;
#3392 = EDGE_LOOP ( 'NONE', ( #14489, #5848, #17476, #6477 ) ) ;
#3393 = ORIENTED_EDGE ( 'NONE', *, *, #17820, .T. ) ;
#3394 = AXIS2_PLACEMENT_3D ( 'NONE', #13069, #11740, #158 ) ;
#3395 = SURFACE_SIDE_STYLE ('',( #14626 ) ) ;
#3396 = CARTESIAN_POINT ( 'NONE',  ( -71.24615306438076345, 126.2399288045637462, 15.00000000000006928 ) ) ;
#3397 = EDGE_LOOP ( 'NONE', ( #5138, #18295, #8550, #1436 ) ) ;
#3398 = EDGE_CURVE ( 'NONE', #6648, #11131, #2731, .T. ) ;
#3399 = AXIS2_PLACEMENT_3D ( 'NONE', #3207, #405, #16097 ) ;
#3400 = AXIS2_PLACEMENT_3D ( 'NONE', #2004, #17440, #4801 ) ;
#3401 = AXIS2_PLACEMENT_3D ( 'NONE', #10322, #16016, #8910 ) ;
#3402 = DIRECTION ( 'NONE',  ( -0.9396926207859097602, 0.3420201433256649937, 1.086737899652991371E-16 ) ) ;
#3403 = CARTESIAN_POINT ( 'NONE',  ( -53.29103256796045684, 73.45256821284057480, 15.00000000000007105 ) ) ;
#3404 = EDGE_LOOP ( 'NONE', ( #13761, #17961, #6229, #8779, #13764 ) ) ;
#3405 = DIRECTION ( 'NONE',  ( -1.000000000000000000, -0.000000000000000000, -0.000000000000000000 ) ) ;
#3406 = VERTEX_POINT ( 'NONE', #8440 ) ;
#3407 = FACE_OUTER_BOUND ( 'NONE', #14814, .T. ) ;
#3408 = FACE_BOUND ( 'NONE', #11172, .T. ) ;
#3409 = VECTOR ( 'NONE', #16033, 1000.000000000000000 ) ;
#3410 = EDGE_CURVE ( 'NONE', #15435, #4264, #6845, .T. ) ;
#3411 = DIRECTION ( 'NONE',  ( 0.000000000000000000, 1.000000000000000000, 0.000000000000000000 ) ) ;
#3412 = AXIS2_PLACEMENT_3D ( 'NONE', #10913, #5088, #10807 ) ;
#3413 = CARTESIAN_POINT ( 'NONE',  ( -78.02975850117498169, -92.35432678654406402, -43.13417664947088070 ) ) ;
#3414 = AXIS2_PLACEMENT_3D ( 'NONE', #4159, #5461, #14082 ) ;
#3415 = EDGE_LOOP ( 'NONE', ( #2438, #5937, #17018 ) ) ;
#3416 = AXIS2_PLACEMENT_3D ( 'NONE', #16162, #9444, #17662 ) ;
#3417 = EDGE_LOOP ( 'NONE', ( #7450, #3027, #10285, #13477 ) ) ;
#3418 = EDGE_CURVE ( 'NONE', #10351, #13411, #5889, .T. ) ;
#3419 = ORIENTED_EDGE ( 'NONE', *, *, #4942, .T. ) ;
#3420 = EDGE_CURVE ( 'NONE', #13598, #16250, #9844, .T. ) ;
#3421 = DIRECTION ( 'NONE',  ( 0.3420201433256663814, -0.9396926207859093161, 0.000000000000000000 ) ) ;
#3422 = CARTESIAN_POINT ( 'NONE',  ( -50.99714023269321217, 75.97988867778809663, -15.00000000000001421 ) ) ;
#3423 = EDGE_CURVE ( 'NONE', #5426, #14435, #2921, .T. ) ;
#3424 = ORIENTED_EDGE ( 'NONE', *, *, #3552, .T. ) ;
#3425 = APPLICATION_PROTOCOL_DEFINITION ( 'draft international standard', 'automotive_design', 1998, #7176 ) ;
#3426 = FACE_OUTER_BOUND ( 'NONE', #17703, .T. ) ;
#3427 = SHAPE_REPRESENTATION_RELATIONSHIP ( 'NONE' , 'NONE' ,  #15047, #2318 ) ;
#3428 = CARTESIAN_POINT ( 'NONE',  ( -71.24615306438070661, 134.7758360152292312, 15.00000000000006928 ) ) ;
#3429 = DIRECTION ( 'NONE',  ( 0.000000000000000000, 1.000000000000000000, 0.000000000000000000 ) ) ;
#3430 = ORIENTED_EDGE ( 'NONE', *, *, #2732, .F. ) ;
#3431 = AXIS2_PLACEMENT_3D ( 'NONE', #2589, #9692, #6880 ) ;
#3432 = LINE ( 'NONE', #14837, #6279 ) ;
#3433 = AXIS2_PLACEMENT_3D ( 'NONE', #16968, #13992, #9681 ) ;
#3434 = CARTESIAN_POINT ( 'NONE',  ( -57.08002265617300708, 84.22855780814606419, 37.50000000000000000 ) ) ;
#3435 = LINE ( 'NONE', #7557, #3451 ) ;
#3436 = VECTOR ( 'NONE', #13841, 1000.000000000000000 ) ;
#3437 = CARTESIAN_POINT ( 'NONE',  ( -67.59262256747319952, 110.5691553257988460, -26.35917033480641436 ) ) ;
#3438 = CARTESIAN_POINT ( 'NONE',  ( -66.00585202009801833, 57.88796029049324687, 25.00000000000000355 ) ) ;
#3439 = VERTEX_POINT ( 'NONE', #1511 ) ;
#3440 = ADVANCED_FACE ( 'NONE', ( #203 ), #7050, .F. ) ;
#3441 = EDGE_CURVE ( 'NONE', #2873, #1167, #14511, .T. ) ;
#3442 = EDGE_CURVE ( 'NONE', #14366, #2307, #6217, .T. ) ;
#3443 = DIRECTION ( 'NONE',  ( 0.000000000000000000, 1.000000000000000000, 0.000000000000000000 ) ) ;
#3444 = CARTESIAN_POINT ( 'NONE',  ( -68.99615306438067819, 142.7668250816626596, -167.1454815528550739 ) ) ;
#3445 = VERTEX_POINT ( 'NONE', #5625 ) ;
#3446 = EDGE_CURVE ( 'NONE', #16773, #8753, #5338, .T. ) ;
#3447 = CARTESIAN_POINT ( 'NONE',  ( -92.59262256747318531, 50.58224449241411236, 25.00000000000000000 ) ) ;
#3448 = EDGE_LOOP ( 'NONE', ( #17964, #7792, #4837, #16368, #8677, #11944, #5495 ) ) ;
#3449 = ORIENTED_EDGE ( 'NONE', *, *, #10923, .F. ) ;
#3450 = EDGE_CURVE ( 'NONE', #15750, #11410, #12843, .T. ) ;
#3451 = VECTOR ( 'NONE', #2028, 1000.000000000000114 ) ;
#3452 = AXIS2_PLACEMENT_3D ( 'NONE', #8102, #13822, #1199 ) ;
#3453 = APPLICATION_CONTEXT ( 'automotive_design' ) ;
#3454 = DIRECTION ( 'NONE',  ( 1.156482317317869999E-16, 0.000000000000000000, 1.000000000000000000 ) ) ;
#3455 = ORIENTED_EDGE ( 'NONE', *, *, #9148, .T. ) ;
#3456 = EDGE_CURVE ( 'NONE', #2549, #14012, #610, .T. ) ;
#3457 = DIRECTION ( 'NONE',  ( 1.000000000000000000, 0.000000000000000000, 5.077734830647302671E-16 ) ) ;
#3458 = DIRECTION ( 'NONE',  ( 0.000000000000000000, 1.734723475976811433E-15, 1.000000000000000000 ) ) ;
#3459 = EDGE_CURVE ( 'NONE', #11848, #583, #1870, .T. ) ;
#3460 = CARTESIAN_POINT ( 'NONE',  ( -48.43547250063686960, 78.72276507608465579, -167.1454815528550739 ) ) ;
#3461 = PLANE ( 'NONE',  #11652 ) ;
#3462 = FACE_OUTER_BOUND ( 'NONE', #7288, .T. ) ;
#3463 = DIRECTION ( 'NONE',  ( 0.000000000000000000, 0.000000000000000000, 1.000000000000000000 ) ) ;
#3464 = ORIENTED_EDGE ( 'NONE', *, *, #7976, .F. ) ;
#3465 = DIRECTION ( 'NONE',  ( 0.000000000000000000, 0.000000000000000000, -1.000000000000000000 ) ) ;
#3466 = CARTESIAN_POINT ( 'NONE',  ( -71.24615306438107609, 13.14259340456380620, 15.00000000000006928 ) ) ;
#3467 = DIRECTION ( 'NONE',  ( -7.442644330182800165E-16, 1.000000000000000000, 0.000000000000000000 ) ) ;
#3468 = ORIENTED_EDGE ( 'NONE', *, *, #7953, .F. ) ;
#3469 = DIRECTION ( 'NONE',  ( 1.000000000000000000, 0.000000000000000000, 0.000000000000000000 ) ) ;
#3470 = LINE ( 'NONE', #1785, #16081 ) ;
#3471 = ORIENTED_EDGE ( 'NONE', *, *, #6167, .F. ) ;
#3472 = VERTEX_POINT ( 'NONE', #15997 ) ;
#3473 = UNCERTAINTY_MEASURE_WITH_UNIT (LENGTH_MEASURE( 1.000000000000000082E-05 ), #2021, 'distance_accuracy_value', 'NONE');
#3474 = DIRECTION ( 'NONE',  ( -5.204170427930409450E-16, 0.000000000000000000, 1.000000000000000000 ) ) ;
#3475 = CARTESIAN_POINT ( 'NONE',  ( -94.45685920050698314, -2.213358015103445098, -167.1454815528550739 ) ) ;
#3476 = DIRECTION ( 'NONE',  ( 0.000000000000000000, 0.000000000000000000, 1.000000000000000000 ) ) ;
#3477 = CARTESIAN_POINT ( 'NONE',  ( -71.24615306438070661, 138.8062994045637311, -167.1454815528550739 ) ) ;
#3478 = EDGE_LOOP ( 'NONE', ( #11382, #11430, #5476, #16623 ) ) ;
#3479 = CARTESIAN_POINT ( 'NONE',  ( -71.24615306438069240, 187.7866419848965052, -15.00000000000001421 ) ) ;
#3480 = DIRECTION ( 'NONE',  ( 0.000000000000000000, 0.000000000000000000, -1.000000000000000000 ) ) ;
#3481 = ORIENTED_EDGE ( 'NONE', *, *, #8702, .T. ) ;
#3482 = DIRECTION ( 'NONE',  ( 0.000000000000000000, 1.000000000000000000, 0.000000000000000000 ) ) ;
#3483 = DIRECTION ( 'NONE',  ( 0.000000000000000000, 1.000000000000000000, 0.000000000000000000 ) ) ;
#3484 = DIRECTION ( 'NONE',  ( 0.3420201433256854218, 0.9396926207859023217, -0.000000000000000000 ) ) ;
#3485 = CARTESIAN_POINT ( 'NONE',  ( -112.9698934257355631, -91.80660034481556409, 8.049308492551670469 ) ) ;
#3486 = ORIENTED_EDGE ( 'NONE', *, *, #18487, .F. ) ;
#3487 = CARTESIAN_POINT ( 'NONE',  ( -68.99615306438072082, 133.3420471316626958, -167.1454815528550739 ) ) ;
#3488 = ORIENTED_EDGE ( 'NONE', *, *, #8590, .T. ) ;
#3489 = CARTESIAN_POINT ( 'NONE',  ( -71.24615306438076345, 122.2094654152292037, 15.00000000000006928 ) ) ;
#3490 = VERTEX_POINT ( 'NONE', #9424 ) ;
#3491 = PRODUCT_DEFINITION ( 'UNKNOWN', '', #14165, #7047 ) ;
#3492 = ORIENTED_EDGE ( 'NONE', *, *, #8170, .F. ) ;
#3493 = ADVANCED_FACE ( 'NONE', ( #17484 ), #13293, .T. ) ;
#3494 = LINE ( 'NONE', #6385, #17763 ) ;
#3495 = DIRECTION ( 'NONE',  ( 1.000000000000000000, -0.000000000000000000, -0.000000000000000000 ) ) ;
#3496 = ORIENTED_EDGE ( 'NONE', *, *, #6981, .F. ) ;
#3497 = CARTESIAN_POINT ( 'NONE',  ( -36.03642545851251100, 84.22855780814606419, 37.50000000000000000 ) ) ;
#3498 = CARTESIAN_POINT ( 'NONE',  ( -107.5926225674731853, 102.8748711238780373, 20.00000000000000355 ) ) ;
#3499 = ORIENTED_EDGE ( 'NONE', *, *, #9626, .F. ) ;
#3500 = CARTESIAN_POINT ( 'NONE',  ( -107.5926225674732137, 117.8748711238780373, 35.00000000000000000 ) ) ;
#3501 = VERTEX_POINT ( 'NONE', #4668 ) ;
#3502 = DIRECTION ( 'NONE',  ( 0.000000000000000000, 0.000000000000000000, 1.000000000000000000 ) ) ;
#3503 = CARTESIAN_POINT ( 'NONE',  ( -57.08002265617300708, 84.22855780814606419, 15.00000000000006928 ) ) ;
#3504 = EDGE_LOOP ( 'NONE', ( #9305, #206, #17313, #14357 ) ) ;
#3505 = DIRECTION ( 'NONE',  ( -1.000000000000000000, 0.000000000000000000, 0.000000000000000000 ) ) ;
#3506 = FACE_OUTER_BOUND ( 'NONE', #7755, .T. ) ;
#3507 = ORIENTED_EDGE ( 'NONE', *, *, #14030, .F. ) ;
#3508 = ORIENTED_EDGE ( 'NONE', *, *, #342, .T. ) ;
#3509 = CARTESIAN_POINT ( 'NONE',  ( -57.08002265617300708, 84.22855780814606419, -15.00000000000001421 ) ) ;
#3510 = CARTESIAN_POINT ( 'NONE',  ( -57.08002265617300708, 84.22855780814606419, 77.50000000000000000 ) ) ;
#3511 = ORIENTED_EDGE ( 'NONE', *, *, #4383, .T. ) ;
#3512 = EDGE_CURVE ( 'NONE', #15291, #17238, #1771, .T. ) ;
#3513 = CARTESIAN_POINT ( 'NONE',  ( -71.24615306438111872, 21.67850061522927518, 15.00000000000006928 ) ) ;
#3514 = DIRECTION ( 'NONE',  ( 0.000000000000000000, 1.000000000000000000, 0.000000000000000000 ) ) ;
#3515 = DIRECTION ( 'NONE',  ( 0.000000000000000000, 0.000000000000000000, 1.000000000000000000 ) ) ;
#3516 = ORIENTED_EDGE ( 'NONE', *, *, #8266, .F. ) ;
#3517 = DIRECTION ( 'NONE',  ( 2.062304371594500494E-16, -1.000000000000000000, 0.000000000000000000 ) ) ;
#3518 = FACE_OUTER_BOUND ( 'NONE', #6492, .T. ) ;
#3519 = CARTESIAN_POINT ( 'NONE',  ( -71.24615306438080609, 107.3903729045637192, 15.00000000000006928 ) ) ;
#3520 = VECTOR ( 'NONE', #1205, 1000.000000000000000 ) ;
#3521 = LINE ( 'NONE', #4833, #18304 ) ;
#3522 = ORIENTED_EDGE ( 'NONE', *, *, #7873, .T. ) ;
#3523 = CARTESIAN_POINT ( 'NONE',  ( -71.24615306438076345, 123.0983361545637109, -167.1454815528550739 ) ) ;
#3524 = CARTESIAN_POINT ( 'NONE',  ( -65.06546592763150727, -95.65021616327639720, 45.05044770573186952 ) ) ;
#3525 = EDGE_CURVE ( 'NONE', #15440, #6184, #10380, .T. ) ;
#3526 = ORIENTED_EDGE ( 'NONE', *, *, #11566, .T. ) ;
#3527 = EDGE_CURVE ( 'NONE', #857, #3086, #11874, .T. ) ;
#3528 = CARTESIAN_POINT ( 'NONE',  ( 95.45835937779683888, -32.62665103886254059, 7.000000000000010658 ) ) ;
#3529 = DIRECTION ( 'NONE',  ( -1.000000000000000000, -0.000000000000000000, -0.000000000000000000 ) ) ;
#3530 = ORIENTED_EDGE ( 'NONE', *, *, #13071, .F. ) ;
#3531 = ORIENTED_EDGE ( 'NONE', *, *, #1076, .T. ) ;
#3532 = VECTOR ( 'NONE', #1591, 1000.000000000000000 ) ;
#3533 = CARTESIAN_POINT ( 'NONE',  ( -73.32517902883354566, 66.64375664990241432, 92.50000000000000000 ) ) ;
#3534 = EDGE_CURVE ( 'NONE', #12444, #12214, #813, .T. ) ;
#3535 = ORIENTED_EDGE ( 'NONE', *, *, #4255, .F. ) ;
#3536 = EDGE_CURVE ( 'NONE', #1454, #8559, #4093, .T. ) ;
#3537 = FACE_OUTER_BOUND ( 'NONE', #6250, .T. ) ;
#3538 = LINE ( 'NONE', #11963, #9954 ) ;
#3539 = LINE ( 'NONE', #3460, #6696 ) ;
#3540 = CARTESIAN_POINT ( 'NONE',  ( -68.99615306438082030, 96.25779118813026969, -15.00000000000001421 ) ) ;
#3541 = LINE ( 'NONE', #2142, #13306 ) ;
#3542 = DIRECTION ( 'NONE',  ( 1.000000000000000000, 0.000000000000000000, 0.000000000000000000 ) ) ;
#3543 = PRODUCT_DEFINITION_SHAPE ( 'NONE', 'NONE',  #18524 ) ;
#3544 = VERTEX_POINT ( 'NONE', #11109 ) ;
#3545 = EDGE_CURVE ( 'NONE', #18444, #4298, #12618, .T. ) ;
#3546 = CARTESIAN_POINT ( 'NONE',  ( -75.16379081051663036, 61.08681906830677377, -23.95122000524899164 ) ) ;
#3547 = FACE_OUTER_BOUND ( 'NONE', #4272, .T. ) ;
#3549 = EDGE_CURVE ( 'NONE', #8849, #14752, #4178, .T. ) ;
#3548 = VECTOR ( 'NONE', #14420, 1000.000000000000000 ) ;
#3550 = ORIENTED_EDGE ( 'NONE', *, *, #13648, .F. ) ;
#3551 = CARTESIAN_POINT ( 'NONE',  ( -71.24615306438103346, 40.52805651522925245, -15.00000000000001421 ) ) ;
#3552 = EDGE_CURVE ( 'NONE', #16418, #10691, #12536, .T. ) ;
#3553 = VERTEX_POINT ( 'NONE', #18496 ) ;
#3554 = EDGE_CURVE ( 'NONE', #17364, #16487, #11014, .T. ) ;
#3555 = ORIENTED_EDGE ( 'NONE', *, *, #6780, .T. ) ;
#3556 = ADVANCED_FACE ( 'NONE', ( #5665 ), #9599, .F. ) ;
#3557 = DIRECTION ( 'NONE',  ( -1.000000000000000000, -0.000000000000000000, -0.000000000000000000 ) ) ;
#3558 = DIRECTION ( 'NONE',  ( 0.000000000000000000, 1.000000000000000000, 0.000000000000000000 ) ) ;
#3559 = VECTOR ( 'NONE', #9971, 1000.000000000000114 ) ;
#3560 = CARTESIAN_POINT ( 'NONE',  ( -68.99615306438067819, 143.3816809381303585, -15.00000000000001421 ) ) ;
#3561 = DIRECTION ( 'NONE',  ( 0.000000000000000000, 1.000000000000000000, 0.000000000000000000 ) ) ;
#3562 = ORIENTED_EDGE ( 'NONE', *, *, #2621, .T. ) ;
#3563 = DIRECTION ( 'NONE',  ( -0.000000000000000000, -0.000000000000000000, -1.000000000000000000 ) ) ;
#3564 = AXIS2_PLACEMENT_3D ( 'NONE', #674, #3563, #6757 ) ;
#3565 = DIRECTION ( 'NONE',  ( 0.000000000000000000, 1.000000000000000000, 0.000000000000000000 ) ) ;
#3566 = VERTEX_POINT ( 'NONE', #17086 ) ;
#3567 = DIRECTION ( 'NONE',  ( -1.000000000000000000, -0.000000000000000000, -0.000000000000000000 ) ) ;
#3568 = LINE ( 'NONE', #1990, #6002 ) ;
#3569 = CARTESIAN_POINT ( 'NONE',  ( -77.62243764337172536, 88.81248391902214223, 56.54393065445481881 ) ) ;
#3570 = CARTESIAN_POINT ( 'NONE',  ( -113.8539578924278288, -92.35432678654406402, 7.309977258218128604 ) ) ;
#3571 = ORIENTED_EDGE ( 'NONE', *, *, #4773, .T. ) ;
#3572 = FACE_OUTER_BOUND ( 'NONE', #9361, .T. ) ;
#3573 = EDGE_LOOP ( 'NONE', ( #10498, #11283, #13309, #15054 ) ) ;
#3574 = CARTESIAN_POINT ( 'NONE',  ( -68.99615306438091977, 73.65178678166269322, -15.00000000000001421 ) ) ;
#3575 = ORIENTED_EDGE ( 'NONE', *, *, #10532, .T. ) ;
#3576 = AXIS2_PLACEMENT_3D ( 'NONE', #1433, #118, #11615 ) ;
#3577 = AXIS2_PLACEMENT_3D ( 'NONE', #13659, #12355, #4954 ) ;
#3578 = ORIENTED_EDGE ( 'NONE', *, *, #244, .F. ) ;
#3579 = DIRECTION ( 'NONE',  ( 0.000000000000000000, 0.000000000000000000, 1.000000000000000000 ) ) ;
#3580 = LINE ( 'NONE', #13515, #13508 ) ;
#3581 = ORIENTED_EDGE ( 'NONE', *, *, #5346, .F. ) ;
#3582 = DIRECTION ( 'NONE',  ( 0.000000000000000000, 0.000000000000000000, 1.000000000000000000 ) ) ;
#3583 = DIRECTION ( 'NONE',  ( -1.000000000000000000, 0.000000000000000000, 0.000000000000000000 ) ) ;
#3584 = EDGE_LOOP ( 'NONE', ( #11012, #6454, #17245, #11816 ) ) ;
#3585 = CARTESIAN_POINT ( 'NONE',  ( -107.5676225674731654, 57.88796029049330372, 26.35917033480641436 ) ) ;
#3586 = CIRCLE ( 'NONE', #15857, 4.600000000000006750 ) ;
#3587 = ORIENTED_EDGE ( 'NONE', *, *, #17055, .F. ) ;
#3588 = AXIS2_PLACEMENT_3D ( 'NONE', #13020, #4737, #13100 ) ;
#3589 = CARTESIAN_POINT ( 'NONE',  ( -92.59262256747318531, 0.3328663868096687350, -25.00000000000000000 ) ) ;
#3590 = FACE_BOUND ( 'NONE', #12304, .T. ) ;
#3591 = LINE ( 'NONE', #9312, #9715 ) ;
#3592 = AXIS2_PLACEMENT_3D ( 'NONE', #11782, #4738, #3176 ) ;
#3593 = CARTESIAN_POINT ( 'NONE',  ( 0.000000000000000000, -111.0842361345572158, 5.654315315325685987 ) ) ;
#3594 = ORIENTED_EDGE ( 'NONE', *, *, #15888, .F. ) ;
#3595 = AXIS2_PLACEMENT_3D ( 'NONE', #1306, #15712, #7181 ) ;
#3596 = VERTEX_POINT ( 'NONE', #1386 ) ;
#3597 = VECTOR ( 'NONE', #426, 1000.000000000000000 ) ;
#3598 = ORIENTED_EDGE ( 'NONE', *, *, #17958, .T. ) ;
#3599 = DIRECTION ( 'NONE',  ( -0.000000000000000000, -0.000000000000000000, -1.000000000000000000 ) ) ;
#3600 = DIRECTION ( 'NONE',  ( 1.156482317317869999E-16, 0.000000000000000000, 1.000000000000000000 ) ) ;
#3601 = VERTEX_POINT ( 'NONE', #8395 ) ;
#3602 = B_SPLINE_CURVE_WITH_KNOTS ( 'NONE', 3,
 ( #18392, #15282, #5277, #10989, #11080, #2471, #1089, #12497, #18191, #4511, #400, #6088, #38, #7245, #11464, #10053, #12966, #2939, #4421, #3124 ),
 .UNSPECIFIED., .F., .F.,
 ( 4, 2, 2, 2, 2, 2, 2, 2, 2, 4 ),
 ( -1.439925654488394098E-05, 0.0006244272253376518481, 0.001263253707220187783, 0.002540906670985255533, 0.003818559634750323065, 0.005096212598515390164, 0.006373865562280457697, 0.007651518526045524363, 0.008929171489810592763, 0.01020682445357565943 ),
 .UNSPECIFIED. ) ;
#3603 = CARTESIAN_POINT ( 'NONE',  ( -107.5926225674731995, 60.58224449241411946, 25.00000000000000000 ) ) ;
#3604 = CARTESIAN_POINT ( 'NONE',  ( -77.09486422618832080, 77.72307496574235586, 66.26442681581322347 ) ) ;
#3605 = CARTESIAN_POINT ( 'NONE',  ( -64.09025127992791226, 117.8748711238780373, 7.000000000000009770 ) ) ;
#3606 = CARTESIAN_POINT ( 'NONE',  ( -57.08002265617300708, 84.22855780814606419, -167.1454815528550739 ) ) ;
#3607 = ORIENTED_EDGE ( 'NONE', *, *, #11354, .F. ) ;
#3608 = EDGE_CURVE ( 'NONE', #11153, #4979, #11030, .T. ) ;
#3609 = AXIS2_PLACEMENT_3D ( 'NONE', #4256, #4346, #17241 ) ;
#3610 = PLANE ( 'NONE',  #8080 ) ;
#3611 = DIRECTION ( 'NONE',  ( 1.000000000000000000, 0.000000000000000000, 3.771137991253923150E-16 ) ) ;
#3612 = PLANE ( 'NONE',  #4637 ) ;
#3613 = DIRECTION ( 'NONE',  ( 0.000000000000000000, 5.551115123125747573E-17, 1.000000000000000000 ) ) ;
#3614 = ORIENTED_EDGE ( 'NONE', *, *, #14205, .F. ) ;
#3615 = VECTOR ( 'NONE', #3483, 1000.000000000000000 ) ;
#3616 = CIRCLE ( 'NONE', #1541, 4.999999999999997335 ) ;
#3617 = CARTESIAN_POINT ( 'NONE',  ( -94.45685920050698314, -47.21335801510345220, -15.00000000000001421 ) ) ;
#3618 = DIRECTION ( 'NONE',  ( -0.000000000000000000, -0.000000000000000000, -1.000000000000000000 ) ) ;
#3619 = ORIENTED_EDGE ( 'NONE', *, *, #6157, .F. ) ;
#3620 = ADVANCED_FACE ( 'NONE', ( #3990 ), #4278, .T. ) ;
#3621 = CARTESIAN_POINT ( 'NONE',  ( -107.5926225674731711, 57.88796029049330372, -22.33417033480641223 ) ) ;
#3622 = CARTESIAN_POINT ( 'NONE',  ( -37.34515446474368616, 76.92303621577349304, 60.78520344204553538 ) ) ;
#3623 = ORIENTED_EDGE ( 'NONE', *, *, #2064, .F. ) ;
#3624 = ORIENTED_EDGE ( 'NONE', *, *, #14967, .F. ) ;
#3625 = VECTOR ( 'NONE', #16749, 1000.000000000000000 ) ;
#3626 = CARTESIAN_POINT ( 'NONE',  ( -68.99615306438109030, 17.71797493813028268, -167.1454815528550739 ) ) ;
#3627 = ORIENTED_EDGE ( 'NONE', *, *, #11797, .T. ) ;
#3628 = VECTOR ( 'NONE', #4692, 1000.000000000000000 ) ;
#3629 = VECTOR ( 'NONE', #6365, 1000.000000000000000 ) ;
#3630 = DIRECTION ( 'NONE',  ( -1.000000000000000000, -0.000000000000000000, -0.000000000000000000 ) ) ;
#3631 = DIRECTION ( 'NONE',  ( 0.000000000000000000, 1.000000000000000000, 0.000000000000000000 ) ) ;
#3632 = CARTESIAN_POINT ( 'NONE',  ( -107.5926225674732137, 117.8748711238780373, 25.00000000000000000 ) ) ;
#3633 = DIRECTION ( 'NONE',  ( -0.000000000000000000, -0.000000000000000000, -1.000000000000000000 ) ) ;
#3634 = DIRECTION ( 'NONE',  ( -1.000000000000000000, 0.000000000000000000, 0.000000000000000000 ) ) ;
#3635 = DIRECTION ( 'NONE',  ( 1.000000000000000000, 0.000000000000000000, 0.000000000000000000 ) ) ;
#3636 = VERTEX_POINT ( 'NONE', #18216 ) ;
#3637 = AXIS2_PLACEMENT_3D ( 'NONE', #18225, #1301, #5584 ) ;
#3638 = DIRECTION ( 'NONE',  ( 0.000000000000000000, 0.000000000000000000, -1.000000000000000000 ) ) ;
#3639 = DIRECTION ( 'NONE',  ( 1.000000000000000000, 1.119176436114069332E-16, 0.000000000000000000 ) ) ;
#3640 = ORIENTED_EDGE ( 'NONE', *, *, #9768, .F. ) ;
#3641 = EDGE_CURVE ( 'NONE', #1745, #12836, #15600, .T. ) ;
#3642 = EDGE_CURVE ( 'NONE', #4254, #8291, #18313, .T. ) ;
#3643 = VECTOR ( 'NONE', #11654, 1000.000000000000000 ) ;
#3644 = DIRECTION ( 'NONE',  ( -1.000000000000000000, -2.978937767313084233E-14, 1.692578276882434470E-16 ) ) ;
#3645 = CIRCLE ( 'NONE', #7537, 10.24900000000001477 ) ;
#3646 = CARTESIAN_POINT ( 'NONE',  ( -71.24615306438074924, 123.0983361545637109, -15.00000000000001421 ) ) ;
#3647 = ORIENTED_EDGE ( 'NONE', *, *, #1800, .T. ) ;
#3648 = EDGE_CURVE ( 'NONE', #10547, #2688, #3849, .T. ) ;
#3649 = EDGE_LOOP ( 'NONE', ( #9182, #9488, #18317, #11993 ) ) ;
#3650 = PRODUCT_DEFINITION_CONTEXT ( 'detailed design', #6188, 'design' ) ;
#3651 = AXIS2_PLACEMENT_3D ( 'NONE', #11076, #8365, #6679 ) ;
#3652 = EDGE_CURVE ( 'NONE', #5943, #10611, #9705, .T. ) ;
#3653 = CARTESIAN_POINT ( 'NONE',  ( -57.08002265617300708, 84.22855780814606419, 15.00000000000006928 ) ) ;
#3654 = CARTESIAN_POINT ( 'NONE',  ( -57.08002265617300708, 84.22855780814606419, -15.00000000000001421 ) ) ;
#3655 = EDGE_CURVE ( 'NONE', #5451, #17731, #8582, .T. ) ;
#3656 = CARTESIAN_POINT ( 'NONE',  ( -65.06546592763099568, -111.0842361345572158, -28.18308811886532084 ) ) ;
#3657 = FACE_OUTER_BOUND ( 'NONE', #13859, .T. ) ;
#3658 = EDGE_CURVE ( 'NONE', #5717, #3274, #3890, .T. ) ;
#3659 = VERTEX_POINT ( 'NONE', #12889 ) ;
#3660 = VECTOR ( 'NONE', #2672, 1000.000000000000000 ) ;
#3661 = DIRECTION ( 'NONE',  ( 6.950654929607132427E-15, 0.000000000000000000, -1.000000000000000000 ) ) ;
#3662 = TOROIDAL_SURFACE ( 'NONE', #17400, 21.04359719766050674, 1.000000000000000000 ) ;
#3663 = DIRECTION ( 'NONE',  ( -0.000000000000000000, -1.000000000000000000, -0.000000000000000000 ) ) ;
#3664 = EDGE_CURVE ( 'NONE', #10905, #14281, #11210, .T. ) ;
#3665 = VERTEX_POINT ( 'NONE', #6994 ) ;
#3666 = CARTESIAN_POINT ( 'NONE',  ( -67.15882256147138207, 111.8146619846916821, 23.31672727879027462 ) ) ;
#3667 = DIRECTION ( 'NONE',  ( 0.000000000000000000, 0.000000000000000000, 1.000000000000000000 ) ) ;
#3668 = CARTESIAN_POINT ( 'NONE',  ( -70.71978124295696944, -111.0842361345572158, -18.23991632971910803 ) ) ;
#3669 = LINE ( 'NONE', #7695, #3350 ) ;
#3670 = VERTEX_POINT ( 'NONE', #8496 ) ;
#3671 = LINE ( 'NONE', #9383, #12559 ) ;
#3672 = EDGE_LOOP ( 'NONE', ( #5389, #609, #2643, #3697 ) ) ;
#3673 = EDGE_CURVE ( 'NONE', #18141, #12144, #11301, .T. ) ;
#3674 = VECTOR ( 'NONE', #2980, 1000.000000000000000 ) ;
#3675 = EDGE_CURVE ( 'NONE', #4742, #7351, #16088, .T. ) ;
#3676 = EDGE_CURVE ( 'NONE', #13750, #7723, #7361, .T. ) ;
#3677 = FACE_OUTER_BOUND ( 'NONE', #6379, .T. ) ;
#3678 = EDGE_LOOP ( 'NONE', ( #13136, #965, #15348, #4080 ) ) ;
#3679 = EDGE_CURVE ( 'NONE', #6562, #1454, #10344, .T. ) ;
#3680 = VECTOR ( 'NONE', #10466, 1000.000000000000000 ) ;
#3681 = AXIS2_PLACEMENT_3D ( 'NONE', #16726, #1043, #8035 ) ;
#3682 = AXIS2_PLACEMENT_3D ( 'NONE', #17936, #9442, #16535 ) ;
#3683 = ORIENTED_EDGE ( 'NONE', *, *, #5261, .T. ) ;
#3684 = CARTESIAN_POINT ( 'NONE',  ( -71.24615306438107609, 28.85055665456374285, -15.00000000000001421 ) ) ;
#3685 = CARTESIAN_POINT ( 'NONE',  ( -92.59262256747321373, 110.5691553257988460, -22.35917033480641791 ) ) ;
#3686 = DIRECTION ( 'NONE',  ( 1.000000000000000000, 0.000000000000000000, 0.000000000000000000 ) ) ;
#3687 = CIRCLE ( 'NONE', #14161, 10.24900000000000055 ) ;
#3688 = VERTEX_POINT ( 'NONE', #16117 ) ;
#3689 = EDGE_CURVE ( 'NONE', #9250, #12214, #15812, .T. ) ;
#3690 = LINE ( 'NONE', #12018, #16151 ) ;
#3691 = EDGE_CURVE ( 'NONE', #10695, #14578, #1649, .T. ) ;
#3692 = CARTESIAN_POINT ( 'NONE',  ( -65.06546592763082515, -96.08423613455721579, -45.05044770573174873 ) ) ;
#3693 = ORIENTED_EDGE ( 'NONE', *, *, #2291, .T. ) ;
#3694 = DIRECTION ( 'NONE',  ( 0.000000000000000000, 0.000000000000000000, 1.000000000000000000 ) ) ;
#3695 =( GEOMETRIC_REPRESENTATION_CONTEXT ( 3 ) GLOBAL_UNCERTAINTY_ASSIGNED_CONTEXT ( ( #2337 ) ) GLOBAL_UNIT_ASSIGNED_CONTEXT ( ( #8875, #1485, #17279 ) ) REPRESENTATION_CONTEXT ( 'NONE', 'WORKASPACE' ) );
#3696 = AXIS2_PLACEMENT_3D ( 'NONE', #4921, #9141, #9502 ) ;
#3697 = ORIENTED_EDGE ( 'NONE', *, *, #14225, .T. ) ;
#3698 = AXIS2_PLACEMENT_3D ( 'NONE', #2954, #14364, #14461 ) ;
#3699 = CARTESIAN_POINT ( 'NONE',  ( -68.99615306438090556, 61.70027203813025807, 15.00000000000006928 ) ) ;
#3700 = CARTESIAN_POINT ( 'NONE',  ( -66.31963392321378592, 109.2426495258444277, 25.00000000000000355 ) ) ;
#3701 = ORIENTED_EDGE ( 'NONE', *, *, #9610, .T. ) ;
#3702 = DIRECTION ( 'NONE',  ( 0.000000000000000000, 0.000000000000000000, 1.000000000000000000 ) ) ;
#3703 = APPLICATION_CONTEXT ( 'automotive_design' ) ;
#3704 = PRESENTATION_LAYER_ASSIGNMENT (  '', '', ( #10581 ) ) ;
#3705 = CARTESIAN_POINT ( 'NONE',  ( -79.28150129717847960, -91.53393135689863414, -41.62626982970579803 ) ) ;
#3706 = EDGE_LOOP ( 'NONE', ( #10881, #13062, #5823, #9646, #13348, #17339 ) ) ;
#3707 = ORIENTED_EDGE ( 'NONE', *, *, #10319, .F. ) ;
#3708 = CIRCLE ( 'NONE', #13274, 4.599999999999992539 ) ;
#3709 = CONICAL_SURFACE ( 'NONE', #16848, 4.025000000000000355, 0.7853981633975870569 ) ;
#3710 = VERTEX_POINT ( 'NONE', #9029 ) ;
#3711 = CARTESIAN_POINT ( 'NONE',  ( -71.24615306438096241, 44.55851990456374523, 15.00000000000006928 ) ) ;
#3712 = CARTESIAN_POINT ( 'NONE',  ( -36.03642545851251100, 84.22855780814606419, 77.50000000000000000 ) ) ;
#3713 = ORIENTED_EDGE ( 'NONE', *, *, #3133, .F. ) ;
#3714 = CARTESIAN_POINT ( 'NONE',  ( -77.35440395286859427, 78.57985073358727846, 67.45754834358830010 ) ) ;
#3715 = CARTESIAN_POINT ( 'NONE',  ( -1.861400446476476622, 12.03450721920232880, 46.70170638485993919 ) ) ;
#3716 = CARTESIAN_POINT ( 'NONE',  ( -57.08002265617300708, 84.22855780814606419, -167.1454815528550739 ) ) ;
#3717 = ORIENTED_EDGE ( 'NONE', *, *, #2652, .F. ) ;
#3718 = FACE_BOUND ( 'NONE', #9187, .T. ) ;
#3719 = CARTESIAN_POINT ( 'NONE',  ( -63.25151023250651150, 93.09943318379590949, 15.00000000000006928 ) ) ;
#3720 = DIRECTION ( 'NONE',  ( 0.000000000000000000, 0.000000000000000000, -1.000000000000000000 ) ) ;
#3721 = CARTESIAN_POINT ( 'NONE',  ( -24.54889247506734762, 50.87908043791564694, 26.71068393001068131 ) ) ;
#3722 = VERTEX_POINT ( 'NONE', #238 ) ;
#3723 = VECTOR ( 'NONE', #12338, 1000.000000000000000 ) ;
#3724 = AXIS2_PLACEMENT_3D ( 'NONE', #2687, #9894, #8499 ) ;
#3725 = AXIS2_PLACEMENT_3D ( 'NONE', #5512, #16718, #9731 ) ;
#3726 = CARTESIAN_POINT ( 'NONE',  ( -71.24615306438116136, 6.859408104563791575, -15.00000000000001421 ) ) ;
#3727 = CARTESIAN_POINT ( 'NONE',  ( -107.5926225674731853, 110.5691553257988460, -30.38417033480641294 ) ) ;
#3728 = ORIENTED_EDGE ( 'NONE', *, *, #16106, .T. ) ;
#3729 = CARTESIAN_POINT ( 'NONE',  ( -68.99615306438070661, 137.0984956381303164, -167.1454815528550739 ) ) ;
#3730 = FILL_AREA_STYLE ('',( #12157 ) ) ;
#3731 = ORIENTED_EDGE ( 'NONE', *, *, #11294, .F. ) ;
#3732 = EDGE_CURVE ( 'NONE', #1119, #13480, #5856, .T. ) ;
#3733 = ORIENTED_EDGE ( 'NONE', *, *, #5841, .T. ) ;
#3734 = CYLINDRICAL_SURFACE ( 'NONE', #15327, 12.50000000000000355 ) ;
#3735 = AXIS2_PLACEMENT_3D ( 'NONE', #13528, #5193, #3505 ) ;
#3736 = ORIENTED_EDGE ( 'NONE', *, *, #3995, .T. ) ;
#3737 = AXIS2_PLACEMENT_3D ( 'NONE', #2325, #8031, #18349 ) ;
#3738 = AXIS2_PLACEMENT_3D ( 'NONE', #12252, #13747, #6735 ) ;
#3739 = CARTESIAN_POINT ( 'NONE',  ( -57.08002265617300708, 84.22855780814606419, 15.00000000000006928 ) ) ;
#3740 = CARTESIAN_POINT ( 'NONE',  ( -73.11430033901579861, 59.62110470154726016, 22.74887301420309882 ) ) ;
#3741 = LINE ( 'NONE', #7849, #10560 ) ;
#3742 = CARTESIAN_POINT ( 'NONE',  ( -47.02742034342072941, 91.65790412808885890, 15.00000000000009592 ) ) ;
#3743 = DIRECTION ( 'NONE',  ( -0.000000000000000000, -0.000000000000000000, 1.000000000000000000 ) ) ;
#3744 = LINE ( 'NONE', #936, #1364 ) ;
#3745 = CARTESIAN_POINT ( 'NONE',  ( -65.06546592763139358, -91.08423613455721579, 28.18308811886540610 ) ) ;
#3746 = ORIENTED_EDGE ( 'NONE', *, *, #2192, .F. ) ;
#3747 = LINE ( 'NONE', #13569, #18017 ) ;
#3748 = FACE_OUTER_BOUND ( 'NONE', #3761, .T. ) ;
#3749 = ORIENTED_EDGE ( 'NONE', *, *, #6518, .F. ) ;
#3750 = DIRECTION ( 'NONE',  ( -0.000000000000000000, -0.000000000000000000, -1.000000000000000000 ) ) ;
#3751 = CARTESIAN_POINT ( 'NONE',  ( -57.08002265617300708, 84.22855780814606419, -167.1454815528550739 ) ) ;
#3752 = ORIENTED_EDGE ( 'NONE', *, *, #8089, .F. ) ;
#3753 = ORIENTED_EDGE ( 'NONE', *, *, #3090, .T. ) ;
#3754 = EDGE_LOOP ( 'NONE', ( #17655, #17248, #10397, #16961 ) ) ;
#3755 = CARTESIAN_POINT ( 'NONE',  ( -47.27059076829218043, 81.25920652595885940, 15.00000000000009592 ) ) ;
#3756 = CARTESIAN_POINT ( 'NONE',  ( -92.59262256747319952, 50.58224449241411236, -25.00000000000000000 ) ) ;
#3757 = CARTESIAN_POINT ( 'NONE',  ( -57.08002265617300708, 84.22855780814606419, 15.00000000000006928 ) ) ;
#3758 = DIRECTION ( 'NONE',  ( -1.000000000000000000, -0.000000000000000000, -0.000000000000000000 ) ) ;
#3759 = ADVANCED_FACE ( 'NONE', ( #10246 ), #14466, .T. ) ;
#3760 = LINE ( 'NONE', #856, #8958 ) ;
#3761 = EDGE_LOOP ( 'NONE', ( #9423, #12681, #13215, #16201 ) ) ;
#3762 = LINE ( 'NONE', #11062, #12623 ) ;
#3763 = LINE ( 'NONE', #10022, #9014 ) ;
#3765 = VERTEX_POINT ( 'NONE', #14629 ) ;
#3764 = DIRECTION ( 'NONE',  ( -1.000000000000000000, -2.826528109797569363E-15, 0.000000000000000000 ) ) ;
#3766 = CARTESIAN_POINT ( 'NONE',  ( -68.99615306438117557, 1.395155831662692192, -167.1454815528550739 ) ) ;
#3767 = CARTESIAN_POINT ( 'NONE',  ( -52.35105328106566702, 95.79950628479642205, -15.00000000000001421 ) ) ;
#3768 = ORIENTED_EDGE ( 'NONE', *, *, #12268, .F. ) ;
#3769 = DIRECTION ( 'NONE',  ( 0.000000000000000000, 0.000000000000000000, 1.000000000000000000 ) ) ;
#3770 = EDGE_LOOP ( 'NONE', ( #9714, #2144, #9930, #5737 ) ) ;
#3771 = EDGE_CURVE ( 'NONE', #4613, #16809, #17341, .T. ) ;
#3772 = ADVANCED_FACE ( 'NONE', ( #16036 ), #17182, .F. ) ;
#3773 = ORIENTED_EDGE ( 'NONE', *, *, #2054, .T. ) ;
#3774 = DIRECTION ( 'NONE',  ( 0.000000000000000000, 0.000000000000000000, 1.000000000000000000 ) ) ;
#3775 = CARTESIAN_POINT ( 'NONE',  ( -70.71978124295696944, -91.08423613455721579, 5.204170427930421283E-15 ) ) ;
#3776 = LINE ( 'NONE', #15567, #2785 ) ;
#3777 = ADVANCED_FACE ( 'NONE', ( #14719 ), #4529, .T. ) ;
#3778 = ORIENTED_EDGE ( 'NONE', *, *, #4784, .F. ) ;
#3779 = PRODUCT_CONTEXT ( 'NONE', #6933, 'mechanical' ) ;
#3780 = EDGE_CURVE ( 'NONE', #4264, #10128, #7159, .T. ) ;
#3781 = EDGE_CURVE ( 'NONE', #10136, #3332, #8763, .T. ) ;
#3782 = DIRECTION ( 'NONE',  ( 1.156482317317869999E-16, 0.000000000000000000, 1.000000000000000000 ) ) ;
#3783 = DIRECTION ( 'NONE',  ( -0.9396926207859097602, 0.3420201433256649381, -4.890320548438455808E-16 ) ) ;
#3784 = VERTEX_POINT ( 'NONE', #4706 ) ;
#3785 = DIRECTION ( 'NONE',  ( 0.9396926207859097602, 0.3420201433256649937, 0.000000000000000000 ) ) ;
#3786 = LINE ( 'NONE', #985, #16178 ) ;
#3787 = ORIENTED_EDGE ( 'NONE', *, *, #15596, .T. ) ;
#3788 = CARTESIAN_POINT ( 'NONE',  ( -75.16338607169024044, 107.3706141836132986, -23.95078896739801522 ) ) ;
#3789 = CARTESIAN_POINT ( 'NONE',  ( -66.02576182061889654, 110.2283017972794141, 25.00000000000000711 ) ) ;
#3790 = ORIENTED_EDGE ( 'NONE', *, *, #255, .F. ) ;
#3791 = EDGE_CURVE ( 'NONE', #9544, #9457, #2975, .T. ) ;
#3792 = PLANE ( 'NONE',  #747 ) ;
#3793 = CARTESIAN_POINT ( 'NONE',  ( -123.4618227840623632, -151.5628872026273086, -57.00000000000000000 ) ) ;
#3794 = ORIENTED_EDGE ( 'NONE', *, *, #12315, .T. ) ;
#3795 = EDGE_CURVE ( 'NONE', #6928, #1519, #10151, .T. ) ;
#3796 = EDGE_CURVE ( 'NONE', #15896, #17894, #3147, .T. ) ;
#3797 = ORIENTED_EDGE ( 'NONE', *, *, #13513, .T. ) ;
#3798 = ORIENTED_EDGE ( 'NONE', *, *, #5433, .T. ) ;
#3799 = LINE ( 'NONE', #7642, #9671 ) ;
#3800 = DIRECTION ( 'NONE',  ( -0.000000000000000000, -0.000000000000000000, -1.000000000000000000 ) ) ;
#3801 = EDGE_CURVE ( 'NONE', #16706, #10794, #15822, .T. ) ;
#3802 = ORIENTED_EDGE ( 'NONE', *, *, #13172, .F. ) ;
#3803 = LINE ( 'NONE', #6600, #575 ) ;
#3804 = CARTESIAN_POINT ( 'NONE',  ( -77.22213323485729575, 78.13360439242252653, 58.12270716872546927 ) ) ;
#3805 = DIRECTION ( 'NONE',  ( 1.156482317317869999E-16, 0.000000000000000000, 1.000000000000000000 ) ) ;
#3806 = CARTESIAN_POINT ( 'NONE',  ( -57.08002265617300708, 84.22855780814606419, 25.00000000000000355 ) ) ;
#3807 = ORIENTED_EDGE ( 'NONE', *, *, #17495, .T. ) ;
#3808 = FACE_OUTER_BOUND ( 'NONE', #14290, .T. ) ;
#3809 = FACE_OUTER_BOUND ( 'NONE', #2592, .T. ) ;
#3810 = SURFACE_STYLE_USAGE ( .BOTH. , #15027 ) ;
#3811 = FACE_OUTER_BOUND ( 'NONE', #10155, .T. ) ;
#3812 = CARTESIAN_POINT ( 'NONE',  ( -21.11045101004114599, 48.70050140195975530, 28.18094419443968235 ) ) ;
#3813 = ORIENTED_EDGE ( 'NONE', *, *, #2874, .F. ) ;
#3814 = DIRECTION ( 'NONE',  ( -1.000000000000000000, 0.000000000000000000, 0.000000000000000000 ) ) ;
#3815 = LINE ( 'NONE', #5114, #5971 ) ;
#3816 = VERTEX_POINT ( 'NONE', #2958 ) ;
#3817 = CARTESIAN_POINT ( 'NONE',  ( -68.99615306438097662, 57.94382353166266597, -15.00000000000001421 ) ) ;
#3818 = ORIENTED_EDGE ( 'NONE', *, *, #13838, .T. ) ;
#3819 = ORIENTED_EDGE ( 'NONE', *, *, #14218, .F. ) ;
#3820 = CARTESIAN_POINT ( 'NONE',  ( -57.08002265617300708, 84.22855780814606419, -2.999999999999999112 ) ) ;
#3821 = VERTEX_POINT ( 'NONE', #8663 ) ;
#3822 = DIRECTION ( 'NONE',  ( 0.000000000000000000, -4.000800291689476871E-17, -1.000000000000000000 ) ) ;
#3823 = CYLINDRICAL_SURFACE ( 'NONE', #8769, 3.999999999999996447 ) ;
#3824 = VECTOR ( 'NONE', #17984, 1000.000000000000000 ) ;
#3825 = DIRECTION ( 'NONE',  ( -0.000000000000000000, -1.000000000000000000, -0.000000000000000000 ) ) ;
#3826 = DIRECTION ( 'NONE',  ( 1.000000000000000000, 0.000000000000000000, 0.000000000000000000 ) ) ;
#3827 = CARTESIAN_POINT ( 'NONE',  ( 5.299999999999998934, 0.000000000000000000, 0.000000000000000000 ) ) ;
#3828 = PLANE ( 'NONE',  #5534 ) ;
#3829 = LINE ( 'NONE', #9824, #9625 ) ;
#3830 = ORIENTED_EDGE ( 'NONE', *, *, #9959, .T. ) ;
#3831 = CARTESIAN_POINT ( 'NONE',  ( -71.24615306438080609, 104.2487802545637408, 15.00000000000006928 ) ) ;
#3832 = CARTESIAN_POINT ( 'NONE',  ( -67.13262496892538422, 91.65790412808873100, -15.00000000000001421 ) ) ;
#3833 = ORIENTED_EDGE ( 'NONE', *, *, #13387, .T. ) ;
#3834 = CARTESIAN_POINT ( 'NONE',  ( -71.24615306438111872, 21.67850061522927518, 15.00000000000006928 ) ) ;
#3835 = CARTESIAN_POINT ( 'NONE',  ( -47.80867013224673912, 89.78028827820993740, -15.00000000000001421 ) ) ;
#3836 = ORIENTED_EDGE ( 'NONE', *, *, #7665, .F. ) ;
#3837 = AXIS2_PLACEMENT_3D ( 'NONE', #3931, #5242, #9543 ) ;
#3838 = VERTEX_POINT ( 'NONE', #14369 ) ;
#3839 = VERTEX_POINT ( 'NONE', #7263 ) ;
#3840 = PRODUCT_DEFINITION_CONTEXT ( 'detailed design', #3703, 'design' ) ;
#3841 = CARTESIAN_POINT ( 'NONE',  ( -60.31105839772099841, 93.95493478196522119, -167.1454815528550739 ) ) ;
#3842 = CARTESIAN_POINT ( 'NONE',  ( -68.99615306438080609, 108.2093059316626693, -15.00000000000001421 ) ) ;
#3843 = CARTESIAN_POINT ( 'NONE',  ( -71.24615306438104767, 19.42577870456378619, 15.00000000000006928 ) ) ;
#3844 = DIRECTION ( 'NONE',  ( 0.9396926207859158664, 0.3420201433256481738, 0.000000000000000000 ) ) ;
#3845 = DIRECTION ( 'NONE',  ( 0.000000000000000000, 0.000000000000000000, 1.000000000000000000 ) ) ;
#3846 = DIRECTION ( 'NONE',  ( -1.000000000000000000, 0.000000000000000000, 0.000000000000000000 ) ) ;
#3847 = B_SPLINE_CURVE_WITH_KNOTS ( 'NONE', 3,
 ( #5520, #5318, #2528, #9532, #1036, #6922, #12649, #15522 ),
 .UNSPECIFIED., .F., .F.,
 ( 4, 2, 2, 4 ),
 ( 0.003797433802554399471, 0.004743183970586228350, 0.005688934138618056795, 0.007580434474681712817 ),
 .UNSPECIFIED. ) ;
#3848 = ORIENTED_EDGE ( 'NONE', *, *, #11899, .T. ) ;
#3849 = CIRCLE ( 'NONE', #17006, 10.24899999999998812 ) ;
#3850 = DIRECTION ( 'NONE',  ( 0.000000000000000000, 0.000000000000000000, -1.000000000000000000 ) ) ;
#3851 = DIRECTION ( 'NONE',  ( -1.000000000000000000, 0.000000000000000000, 0.000000000000000000 ) ) ;
#3853 = ORIENTED_EDGE ( 'NONE', *, *, #14093, .T. ) ;
#3852 = FACE_OUTER_BOUND ( 'NONE', #10007, .T. ) ;
#3854 = CARTESIAN_POINT ( 'NONE',  ( -68.99615306438076345, 115.1073470881302541, -15.00000000000001421 ) ) ;
#3855 = DIRECTION ( 'NONE',  ( 0.000000000000000000, 0.000000000000000000, 1.000000000000000000 ) ) ;
#3856 = ORIENTED_EDGE ( 'NONE', *, *, #8372, .F. ) ;
#3857 = ORIENTED_EDGE ( 'NONE', *, *, #3459, .F. ) ;
#3858 = EDGE_CURVE ( 'NONE', #9128, #8646, #7451, .T. ) ;
#3859 = VECTOR ( 'NONE', #14982, 1000.000000000000000 ) ;
#3860 = VERTEX_POINT ( 'NONE', #11571 ) ;
#3861 = CIRCLE ( 'NONE', #4787, 26.04359719766049608 ) ;
#3862 =( NAMED_UNIT ( * ) PLANE_ANGLE_UNIT ( ) SI_UNIT ( $, .RADIAN. ) );
#3863 = DIRECTION ( 'NONE',  ( 0.9396926207859171987, 0.3420201433256445100, 4.890320548438495251E-16 ) ) ;
#3864 = CARTESIAN_POINT ( 'NONE',  ( -102.4618227840623774, 0.000000000000000000, 36.00000000000000711 ) ) ;
#3865 = ORIENTED_EDGE ( 'NONE', *, *, #17928, .F. ) ;
#3866 = ITEM_DEFINED_TRANSFORMATION ( 'NONE', 'NONE', #6990,  #16217 ) ;
#3867 = DIRECTION ( 'NONE',  ( 0.000000000000000000, 0.000000000000000000, 1.000000000000000000 ) ) ;
#3868 = EDGE_CURVE ( 'NONE', #11029, #4091, #15106, .T. ) ;
#3869 = CARTESIAN_POINT ( 'NONE',  ( -71.24615306438073503, 128.4926507152292459, -15.00000000000001421 ) ) ;
#3870 = EDGE_LOOP ( 'NONE', ( #6331, #1737, #3798, #5123 ) ) ;
#3871 = DIRECTION ( 'NONE',  ( -1.000000000000000000, 0.000000000000000000, 0.000000000000000000 ) ) ;
#3872 = DIRECTION ( 'NONE',  ( -0.000000000000000000, -0.000000000000000000, 1.000000000000000000 ) ) ;
#3873 = ORIENTED_EDGE ( 'NONE', *, *, #14964, .T. ) ;
#3874 = AXIS2_PLACEMENT_3D ( 'NONE', #1179, #4081, #14088 ) ;
#3875 = DIRECTION ( 'NONE',  ( -1.000000000000000000, -1.218656359355351063E-14, 1.692578276882432005E-16 ) ) ;
#3876 = CARTESIAN_POINT ( 'NONE',  ( -57.08002265617300708, 84.22855780814606419, 15.00000000000006928 ) ) ;
#3877 = CARTESIAN_POINT ( 'NONE',  ( -68.99615306438111872, 7.678341131662685726, 15.00000000000006928 ) ) ;
#3878 = EDGE_CURVE ( 'NONE', #9354, #14934, #13422, .T. ) ;
#3879 = EDGE_CURVE ( 'NONE', #14168, #15468, #4180, .T. ) ;
#3880 = DIRECTION ( 'NONE',  ( 0.000000000000000000, 0.000000000000000000, 1.000000000000000000 ) ) ;
#3881 = EDGE_LOOP ( 'NONE', ( #3378, #11988, #4276, #11600, #8921 ) ) ;
#3882 = EDGE_CURVE ( 'NONE', #3060, #14435, #7171, .T. ) ;
#3883 = ORIENTED_EDGE ( 'NONE', *, *, #5854, .F. ) ;
#3884 = AXIS2_PLACEMENT_3D ( 'NONE', #12392, #2352, #18175 ) ;
#3885 = CARTESIAN_POINT ( 'NONE',  ( -35.92682688279126779, 73.26749283227019305, 97.49999999999998579 ) ) ;
#3886 = LINE ( 'NONE', #18308, #15661 ) ;
#3887 = EDGE_LOOP ( 'NONE', ( #16536, #6308, #10227, #10193 ) ) ;
#3888 = VECTOR ( 'NONE', #15909, 1000.000000000000000 ) ;
#3889 = CARTESIAN_POINT ( 'NONE',  ( -53.39175999306721110, 74.07097899412303832, 15.00000000000006928 ) ) ;
#3890 = LINE ( 'NONE', #18413, #4445 ) ;
#3891 = VECTOR ( 'NONE', #14043, 1000.000000000000000 ) ;
#3892 = LINE ( 'NONE', #624, #9966 ) ;
#3893 = ADVANCED_FACE ( 'NONE', ( #18398, #15289 ), #2671, .F. ) ;
#3894 = DIRECTION ( 'NONE',  ( -0.000000000000000000, -0.000000000000000000, 1.000000000000000000 ) ) ;
#3895 = ORIENTED_EDGE ( 'NONE', *, *, #8390, .F. ) ;
#3896 = DIRECTION ( 'NONE',  ( -0.9396926207859068736, 0.3420201433256725987, -4.890320548438441017E-16 ) ) ;
#3897 = CARTESIAN_POINT ( 'NONE',  ( -46.36441787118067026, 82.83016482797245317, 15.00000000000009592 ) ) ;
#3898 = DIRECTION ( 'NONE',  ( 1.000000000000000000, 0.000000000000000000, 0.000000000000000000 ) ) ;
#3899 = ADVANCED_FACE ( 'NONE', ( #15397 ), #2479, .T. ) ;
#3900 = CARTESIAN_POINT ( 'NONE',  ( -71.24615306438106188, 37.38646386522923137, -167.1454815528550739 ) ) ;
#3901 = CARTESIAN_POINT ( 'NONE',  ( -5.341607757298564074, 34.93162786869717706, 36.42599446819355791 ) ) ;
#3902 = ORIENTED_EDGE ( 'NONE', *, *, #10802, .T. ) ;
#3903 = VECTOR ( 'NONE', #14581, 1000.000000000000114 ) ;
#3904 = PLANE ( 'NONE',  #6103 ) ;
#3905 = CARTESIAN_POINT ( 'NONE',  ( -61.37143594624264153, -91.24992749556382421, 40.65007029793621030 ) ) ;
#3906 = CIRCLE ( 'NONE', #26, 4.025000000000000355 ) ;
#3907 = EDGE_CURVE ( 'NONE', #3636, #4573, #8287, .T. ) ;
#3908 = ADVANCED_FACE ( 'NONE', ( #16885 ), #16779, .F. ) ;
#3909 = LINE ( 'NONE', #12733, #11929 ) ;
#3910 = AXIS2_PLACEMENT_3D ( 'NONE', #10079, #7365, #7531 ) ;
#3911 = ORIENTED_EDGE ( 'NONE', *, *, #15912, .F. ) ;
#3912 = CIRCLE ( 'NONE', #8948, 40.40389983439752086 ) ;
#3913 = ORIENTED_EDGE ( 'NONE', *, *, #2524, .F. ) ;
#3914 = CARTESIAN_POINT ( 'NONE',  ( 8.065334786029138841E-14, -5.788408252968062051, -2.974182810908597041 ) ) ;
#3915 = AXIS2_PLACEMENT_3D ( 'NONE', #14702, #7413, #1796 ) ;
#3916 = ORIENTED_EDGE ( 'NONE', *, *, #5236, .F. ) ;
#3917 = FACE_OUTER_BOUND ( 'NONE', #6327, .T. ) ;
#3918 = CARTESIAN_POINT ( 'NONE',  ( -68.99615306438080609, 105.0677132816627051, 15.00000000000006928 ) ) ;
#3919 = CARTESIAN_POINT ( 'NONE',  ( -66.20510745737880143, 58.30955781107306279, -28.00000000000000355 ) ) ;
#3920 = PLANE ( 'NONE',  #5070 ) ;
#3921 = AXIS2_PLACEMENT_3D ( 'NONE', #16023, #10138, #2944 ) ;
#3922 = DIRECTION ( 'NONE',  ( 0.000000000000000000, 0.000000000000000000, 1.000000000000000000 ) ) ;
#3923 = CARTESIAN_POINT ( 'NONE',  ( -36.44155368744862500, 56.74635804676027107, -2.999999999999999112 ) ) ;
#3924 = ORIENTED_EDGE ( 'NONE', *, *, #16449, .T. ) ;
#3925 = EDGE_CURVE ( 'NONE', #6726, #3490, #16396, .T. ) ;
#3926 = CARTESIAN_POINT ( 'NONE',  ( -71.24615306438109030, 28.85055665456373575, -15.00000000000001421 ) ) ;
#3927 = LINE ( 'NONE', #2246, #15558 ) ;
#3928 = ORIENTED_EDGE ( 'NONE', *, *, #15817, .T. ) ;
#3929 = AXIS2_PLACEMENT_3D ( 'NONE', #14428, #7317, #9763 ) ;
#3930 = DIRECTION ( 'NONE',  ( 0.9396926207859185309, 0.3420201433256406798, 4.890320548438501168E-16 ) ) ;
#3931 = CARTESIAN_POINT ( 'NONE',  ( 56.85086857400936822, 84.22855780814606419, 62.50000000000001421 ) ) ;
#3932 = ORIENTED_EDGE ( 'NONE', *, *, #6255, .T. ) ;
#3933 = ORIENTED_EDGE ( 'NONE', *, *, #792, .T. ) ;
#3934 = CIRCLE ( 'NONE', #14396, 10.24900000000000055 ) ;
#3935 = AXIS2_PLACEMENT_3D ( 'NONE', #9084, #2050, #3635 ) ;
#3936 = VERTEX_POINT ( 'NONE', #10996 ) ;
#3937 = CARTESIAN_POINT ( 'NONE',  ( -107.5926225674731711, 57.88796029049330372, -26.35917033480641436 ) ) ;
#3938 = CARTESIAN_POINT ( 'NONE',  ( -68.99615306438100504, 42.23586028166270978, -15.00000000000001421 ) ) ;
#3939 = DIRECTION ( 'NONE',  ( 0.000000000000000000, 0.000000000000000000, 1.000000000000000000 ) ) ;
#3940 = LINE ( 'NONE', #12380, #8150 ) ;
#3941 = AXIS2_PLACEMENT_3D ( 'NONE', #18324, #8105, #5493 ) ;
#3942 = DIRECTION ( 'NONE',  ( 0.000000000000000000, 0.4999999999999999445, -0.8660254037844387076 ) ) ;
#3943 = FACE_OUTER_BOUND ( 'NONE', #3448, .T. ) ;
#3944 = APPLICATION_CONTEXT ( 'automotive_design' ) ;
#3945 = ORIENTED_EDGE ( 'NONE', *, *, #13961, .F. ) ;
#3946 = DIRECTION ( 'NONE',  ( 1.000000000000000000, 0.000000000000000000, 0.000000000000000000 ) ) ;
#3947 = CARTESIAN_POINT ( 'NONE',  ( -92.59262256747319952, 50.58224449241410525, 15.00000000000005862 ) ) ;
#3949 = ORIENTED_EDGE ( 'NONE', *, *, #17366, .F. ) ;
#3948 = CARTESIAN_POINT ( 'NONE',  ( -77.53399986885767703, 89.18779308299872355, 68.14733228818110433 ) ) ;
#3950 = DIRECTION ( 'NONE',  ( 0.000000000000000000, 1.000000000000000000, 0.000000000000000000 ) ) ;
#3951 = VECTOR ( 'NONE', #7908, 1000.000000000000000 ) ;
#3952 = FACE_OUTER_BOUND ( 'NONE', #8891, .T. ) ;
#3953 = ORIENTED_EDGE ( 'NONE', *, *, #15339, .F. ) ;
#3954 = DIRECTION ( 'NONE',  ( 0.000000000000000000, 1.000000000000000000, -0.000000000000000000 ) ) ;
#3955 = VERTEX_POINT ( 'NONE', #12506 ) ;
#3956 = EDGE_CURVE ( 'NONE', #17138, #4389, #18218, .T. ) ;
#3957 = ORIENTED_EDGE ( 'NONE', *, *, #4008, .F. ) ;
#3958 = VECTOR ( 'NONE', #10997, 1000.000000000000000 ) ;
#3959 = AXIS2_PLACEMENT_3D ( 'NONE', #14352, #7416, #1540 ) ;
#3960 = CARTESIAN_POINT ( 'NONE',  ( -71.24615306438106188, 34.24487121522926003, 15.00000000000006928 ) ) ;
#3961 = CARTESIAN_POINT ( 'NONE',  ( -71.24615306438070661, 135.6647067545637242, 15.00000000000006928 ) ) ;
#3962 = ORIENTED_EDGE ( 'NONE', *, *, #15355, .F. ) ;
#3963 = APPLICATION_PROTOCOL_DEFINITION ( 'draft international standard', 'automotive_design', 1998, #8738 ) ;
#3964 = DIRECTION ( 'NONE',  ( 0.000000000000000000, 0.000000000000000000, 1.000000000000000000 ) ) ;
#3965 = CARTESIAN_POINT ( 'NONE',  ( -45.85876501399108207, 78.72098330317804482, 15.00000000000006928 ) ) ;
#3966 = ORIENTED_EDGE ( 'NONE', *, *, #12235, .F. ) ;
#3967 = AXIS2_PLACEMENT_3D ( 'NONE', #3477, #9191, #14881 ) ;
#3968 = CARTESIAN_POINT ( 'NONE',  ( -57.08002265617300708, 84.22855780814606419, 37.50000000000000000 ) ) ;
#3969 = CARTESIAN_POINT ( 'NONE',  ( -46.89970808030100358, 83.04399200740388665, 15.00000000000006928 ) ) ;
#3970 = DIRECTION ( 'NONE',  ( 1.000000000000000000, 0.000000000000000000, 0.000000000000000000 ) ) ;
#3971 = ORIENTED_EDGE ( 'NONE', *, *, #16066, .T. ) ;
#3972 = CARTESIAN_POINT ( 'NONE',  ( -76.14791583990366064, 106.5656527319057147, -26.51439991379068672 ) ) ;
#3973 = CARTESIAN_POINT ( 'NONE',  ( -38.09490121289055509, 73.26749283227019305, 102.5000000000000000 ) ) ;
#3974 = VERTEX_POINT ( 'NONE', #5365 ) ;
#3975 = AXIS2_PLACEMENT_3D ( 'NONE', #12078, #13301, #3638 ) ;
#3976 = CARTESIAN_POINT ( 'NONE',  ( -71.24615306438066398, 145.0894847045637732, -15.00000000000001421 ) ) ;
#3977 = AXIS2_PLACEMENT_3D ( 'NONE', #9379, #7880, #2348 ) ;
#3978 = CARTESIAN_POINT ( 'NONE',  ( -66.13756031549399950, 56.29129655451910708, -26.34212773717771583 ) ) ;
#3979 = ORIENTED_EDGE ( 'NONE', *, *, #16236, .F. ) ;
#3980 = ORIENTED_EDGE ( 'NONE', *, *, #5034, .T. ) ;
#3981 = CIRCLE ( 'NONE', #13844, 4.600000000000006750 ) ;
#3982 = ADVANCED_FACE ( 'NONE', ( #18111 ), #308, .T. ) ;
#3983 = DIRECTION ( 'NONE',  ( 1.000000000000000000, 0.000000000000000000, 0.000000000000000000 ) ) ;
#3984 = LINE ( 'NONE', #2782, #18354 ) ;
#3985 = DIRECTION ( 'NONE',  ( -1.000000000000000000, 0.000000000000000000, 0.000000000000000000 ) ) ;
#3986 = ORIENTED_EDGE ( 'NONE', *, *, #1269, .F. ) ;
#3987 = AXIS2_PLACEMENT_3D ( 'NONE', #17200, #1574, #17541 ) ;
#3988 = CIRCLE ( 'NONE', #13851, 4.400000000000027889 ) ;
#3989 = CARTESIAN_POINT ( 'NONE',  ( -42.53669312409158465, -111.0842361345572158, 5.654315315325685987 ) ) ;
#3991 = CIRCLE ( 'NONE', #10264, 4.999999999999998224 ) ;
#3990 = FACE_OUTER_BOUND ( 'NONE', #2827, .T. ) ;
#3992 = CARTESIAN_POINT ( 'NONE',  ( -57.08002265617300708, 84.22855780814606419, -15.00000000000001421 ) ) ;
#3993 = DIRECTION ( 'NONE',  ( -1.000000000000000000, 0.000000000000000000, 0.000000000000000000 ) ) ;
#3994 = ORIENTED_EDGE ( 'NONE', *, *, #12676, .F. ) ;
#3995 = EDGE_CURVE ( 'NONE', #10484, #12065, #5915, .T. ) ;
#3996 = CARTESIAN_POINT ( 'NONE',  ( -100.4870060002411805, -151.5628872026273086, 57.00000000000000000 ) ) ;
#3997 = DIRECTION ( 'NONE',  ( 0.9396926207859084279, 0.3420201433256686574, 0.000000000000000000 ) ) ;
#3998 =( LENGTH_UNIT ( ) NAMED_UNIT ( * ) SI_UNIT ( .MILLI., .METRE. ) );
#3999 = EDGE_CURVE ( 'NONE', #10310, #15702, #1543, .T. ) ;
#4000 = DIRECTION ( 'NONE',  ( 1.156482317317869999E-16, 0.000000000000000000, 1.000000000000000000 ) ) ;
#4001 = DIRECTION ( 'NONE',  ( -0.9396926207859093161, 0.3420201433256661594, 0.000000000000000000 ) ) ;
#4002 = ORIENTED_EDGE ( 'NONE', *, *, #16212, .T. ) ;
#4003 = AXIS2_PLACEMENT_3D ( 'NONE', #11482, #4702, #234 ) ;
#4004 = CARTESIAN_POINT ( 'NONE',  ( -68.99615306438091977, 77.40823528813029952, -167.1454815528550739 ) ) ;
#4005 = PLANE ( 'NONE',  #14942 ) ;
#4006 = VECTOR ( 'NONE', #13324, 1000.000000000000000 ) ;
#4007 = CYLINDRICAL_SURFACE ( 'NONE', #5386, 4.599999999999992539 ) ;
#4008 = EDGE_CURVE ( 'NONE', #8703, #8868, #4519, .T. ) ;
#4009 = VECTOR ( 'NONE', #1215, 1000.000000000000000 ) ;
#4010 = CARTESIAN_POINT ( 'NONE',  ( -36.49606879131744108, 79.84943054288081044, 56.40631363092040829 ) ) ;
#4011 = ORIENTED_EDGE ( 'NONE', *, *, #2838, .T. ) ;
#4012 = VECTOR ( 'NONE', #12560, 999.9999999999998863 ) ;
#4013 = ADVANCED_FACE ( 'NONE', ( #14276 ), #8474, .T. ) ;
#4014 = ORIENTED_EDGE ( 'NONE', *, *, #4376, .F. ) ;
#4015 = ADVANCED_FACE ( 'NONE', ( #6004 ), #11379, .T. ) ;
#4016 = DIRECTION ( 'NONE',  ( -0.000000000000000000, -0.000000000000000000, -1.000000000000000000 ) ) ;
#4017 = ORIENTED_EDGE ( 'NONE', *, *, #2067, .T. ) ;
#4018 = CARTESIAN_POINT ( 'NONE',  ( -67.59262256747317110, 56.80567558672318995, 22.50837044127973030 ) ) ;
#4019 = LINE ( 'NONE', #13939, #13536 ) ;
#4020 = CARTESIAN_POINT ( 'NONE',  ( -98.90286936182239685, -91.08423613455721579, 5.654315315325477265 ) ) ;
#4021 = VERTEX_POINT ( 'NONE', #11560 ) ;
#4022 = CONICAL_SURFACE ( 'NONE', #14477, 4.025000000000000355, 0.7853981633974482790 ) ;
#4023 = ADVANCED_FACE ( 'NONE', ( #17330 ), #1715, .T. ) ;
#4024 = EDGE_CURVE ( 'NONE', #7404, #16572, #17020, .T. ) ;
#4025 = CARTESIAN_POINT ( 'NONE',  ( -68.99615306438107609, 17.71797493813027558, -15.00000000000001421 ) ) ;
#4026 = AXIS2_PLACEMENT_3D ( 'NONE', #4095, #1294, #12719 ) ;
#4027 = EDGE_CURVE ( 'NONE', #14163, #4979, #1453, .T. ) ;
#4028 = DIRECTION ( 'NONE',  ( 0.000000000000000000, -1.000000000000000000, 4.000800291689476254E-17 ) ) ;
#4029 = CYLINDRICAL_SURFACE ( 'NONE', #17467, 12.49999999999999645 ) ;
#4030 = AXIS2_PLACEMENT_3D ( 'NONE', #6837, #4132, #11260 ) ;
#4031 = DIRECTION ( 'NONE',  ( 0.000000000000000000, 0.000000000000000000, 1.000000000000000000 ) ) ;
#4032 = PRODUCT_DEFINITION_SHAPE ( 'NONE', 'NONE',  #18530 ) ;
#4033 = ORIENTED_EDGE ( 'NONE', *, *, #4271, .T. ) ;
#4034 = ADVANCED_FACE ( 'NONE', ( #18484 ), #12974, .F. ) ;
#4035 = CARTESIAN_POINT ( 'NONE',  ( -52.55467279550843784, 75.03273214436886462, -15.00000000000001421 ) ) ;
#4036 = ORIENTED_EDGE ( 'NONE', *, *, #1052, .T. ) ;
#4037 = B_SPLINE_CURVE_WITH_KNOTS ( 'NONE', 3,
 ( #13562, #11138, #11035, #5128, #752, #6631, #12540, #16829 ),
 .UNSPECIFIED., .F., .F.,
 ( 4, 2, 2, 4 ),
 ( 0.01670317819300424014, 0.01709299363389421220, 0.01748280907478418772, 0.01826243995656414570 ),
 .UNSPECIFIED. ) ;
#4038 = EDGE_CURVE ( 'NONE', #715, #6290, #9548, .T. ) ;
#4039 = VECTOR ( 'NONE', #2934, 1000.000000000000000 ) ;
#4040 = CARTESIAN_POINT ( 'NONE',  ( -107.5926225674731711, 65.58224449241410525, -20.00000000000000355 ) ) ;
#4041 = CARTESIAN_POINT ( 'NONE',  ( -109.6936274348540508, -91.08423613455721579, 10.65431531532540177 ) ) ;
#4042 = ORIENTED_EDGE ( 'NONE', *, *, #9626, .T. ) ;
#4043 = ORIENTED_EDGE ( 'NONE', *, *, #5121, .T. ) ;
#4044 = CIRCLE ( 'NONE', #15075, 4.599999999999992539 ) ;
#4045 = AXIS2_PLACEMENT_3D ( 'NONE', #5357, #8370, #11465 ) ;
#4046 = EDGE_CURVE ( 'NONE', #3566, #10531, #17246, .T. ) ;
#4047 = AXIS2_PLACEMENT_3D ( 'NONE', #4468, #10181, #8789 ) ;
#4048 = EDGE_CURVE ( 'NONE', #2327, #7640, #8956, .T. ) ;
#4049 = ORIENTED_EDGE ( 'NONE', *, *, #15900, .T. ) ;
#4050 = LINE ( 'NONE', #11340, #9112 ) ;
#4051 = FACE_OUTER_BOUND ( 'NONE', #3584, .T. ) ;
#4052 = DIRECTION ( 'NONE',  ( -1.000000000000000000, 0.000000000000000000, 0.000000000000000000 ) ) ;
#4053 = CARTESIAN_POINT ( 'NONE',  ( -68.99615306438111872, 13.96152643166267993, -167.1454815528550739 ) ) ;
#4054 = CARTESIAN_POINT ( 'NONE',  ( -49.26569365422058411, 90.86016871721223254, -15.00000000000001421 ) ) ;
#4055 = CARTESIAN_POINT ( 'NONE',  ( -71.24615306438097662, 60.26648315456372984, -167.1454815528550739 ) ) ;
#4056 = ADVANCED_FACE ( 'NONE', ( #15680 ), #8357, .T. ) ;
#4057 = ORIENTED_EDGE ( 'NONE', *, *, #5828, .F. ) ;
#4058 = VECTOR ( 'NONE', #1883, 1000.000000000000000 ) ;
#4059 = DIRECTION ( 'NONE',  ( 0.000000000000000000, -0.8660254037844381525, -0.5000000000000008882 ) ) ;
#4060 = ORIENTED_EDGE ( 'NONE', *, *, #7425, .T. ) ;
#4061 = LINE ( 'NONE', #3854, #8143 ) ;
#4062 = AXIS2_PLACEMENT_3D ( 'NONE', #18224, #16806, #15311 ) ;
#4063 = AXIS2_PLACEMENT_3D ( 'NONE', #14838, #17747, #732 ) ;
#4064 = LINE ( 'NONE', #18087, #292 ) ;
#4065 = ORIENTED_EDGE ( 'NONE', *, *, #15986, .T. ) ;
#4066 = DIRECTION ( 'NONE',  ( 1.000000000000000000, 0.000000000000000000, 0.000000000000000000 ) ) ;
#4067 = EDGE_LOOP ( 'NONE', ( #11165, #1388, #11959, #17761 ) ) ;
#4068 = ORIENTED_EDGE ( 'NONE', *, *, #15071, .T. ) ;
#4069 = VECTOR ( 'NONE', #16024, 1000.000000000000000 ) ;
#4070 = LINE ( 'NONE', #5732, #4606 ) ;
#4071 = PLANE ( 'NONE',  #1329 ) ;
#4072 = CARTESIAN_POINT ( 'NONE',  ( -71.24615306438099083, 50.84170520456371634, -15.00000000000001421 ) ) ;
#4073 = VERTEX_POINT ( 'NONE', #8570 ) ;
#4074 = VERTEX_POINT ( 'NONE', #15845 ) ;
#4075 = LINE ( 'NONE', #15478, #7216 ) ;
#4076 = ORIENTED_EDGE ( 'NONE', *, *, #11481, .F. ) ;
#4077 = LINE ( 'NONE', #11085, #6590 ) ;
#4078 = CARTESIAN_POINT ( 'NONE',  ( -71.24615306438100504, 49.95283446522918780, 15.00000000000006928 ) ) ;
#4079 = CARTESIAN_POINT ( 'NONE',  ( 5.233202738124664855, -111.0842361345572158, 57.00000000000000000 ) ) ;
#4080 = ORIENTED_EDGE ( 'NONE', *, *, #5364, .F. ) ;
#4081 = DIRECTION ( 'NONE',  ( 0.000000000000000000, 0.000000000000000000, -1.000000000000000000 ) ) ;
#4082 = CARTESIAN_POINT ( 'NONE',  ( -76.06514409945376087, 73.26749283226919829, 102.5000000000000000 ) ) ;
#4084 = ORIENTED_EDGE ( 'NONE', *, *, #1074, .T. ) ;
#4083 = EDGE_CURVE ( 'NONE', #17985, #16652, #4351, .T. ) ;
#4085 = PLANE ( 'NONE',  #761 ) ;
#4086 = ADVANCED_FACE ( 'NONE', ( #11730 ), #17421, .T. ) ;
#4087 = DIRECTION ( 'NONE',  ( 0.000000000000000000, 1.000000000000000000, 0.000000000000000000 ) ) ;
#4088 = VERTEX_POINT ( 'NONE', #13061 ) ;
#4089 = ORIENTED_EDGE ( 'NONE', *, *, #4353, .T. ) ;
#4090 = DIRECTION ( 'NONE',  ( -1.000000000000000000, 0.000000000000000000, 0.000000000000000000 ) ) ;
#4091 = VERTEX_POINT ( 'NONE', #6277 ) ;
#4092 = CARTESIAN_POINT ( 'NONE',  ( -127.5926225674731995, 47.87487112387803023, -15.00000000000000355 ) ) ;
#4093 = LINE ( 'NONE', #1106, #11914 ) ;
#4094 = DIRECTION ( 'NONE',  ( -1.000000000000000000, 0.000000000000000000, 0.000000000000000000 ) ) ;
#4095 = CARTESIAN_POINT ( 'NONE',  ( -57.08002265617300708, 84.22855780814606419, 15.00000000000006928 ) ) ;
#4096 = ORIENTED_EDGE ( 'NONE', *, *, #8223, .F. ) ;
#4097 = CARTESIAN_POINT ( 'NONE',  ( -71.24615306438080609, 106.5015021652292404, -15.00000000000001421 ) ) ;
#4098 = CARTESIAN_POINT ( 'NONE',  ( -53.44605150580733266, 72.26844686893191749, -15.00000000000001421 ) ) ;
#4099 = CARTESIAN_POINT ( 'NONE',  ( -75.58277579834157223, 107.0370988044063267, 24.46269018718348320 ) ) ;
#4100 = CARTESIAN_POINT ( 'NONE',  ( -7.851504758905779369, 22.18492356653273134, -42.64945817991924315 ) ) ;
#4101 = DIRECTION ( 'NONE',  ( 1.000000000000000000, 0.000000000000000000, 0.000000000000000000 ) ) ;
#4102 = EDGE_LOOP ( 'NONE', ( #511, #3424, #18298, #7956 ) ) ;
#4103 = DIRECTION ( 'NONE',  ( 0.000000000000000000, 1.000000000000000000, 0.000000000000000000 ) ) ;
#4104 = CARTESIAN_POINT ( 'NONE',  ( -68.99615306438074924, 120.7756765316626542, -15.00000000000001421 ) ) ;
#4105 = DIRECTION ( 'NONE',  ( 0.000000000000000000, 0.000000000000000000, 1.000000000000000000 ) ) ;
#4106 = CARTESIAN_POINT ( 'NONE',  ( -68.99615306438103346, 32.81108233166271759, 15.00000000000006928 ) ) ;
#4107 = ORIENTED_EDGE ( 'NONE', *, *, #13378, .T. ) ;
#4108 = ORIENTED_EDGE ( 'NONE', *, *, #3882, .T. ) ;
#4109 = EDGE_CURVE ( 'NONE', #16062, #13980, #4884, .T. ) ;
#4110 = CARTESIAN_POINT ( 'NONE',  ( 0.000000000000000000, 0.000000000000000000, -35.00000000000000000 ) ) ;
#4111 = ORIENTED_EDGE ( 'NONE', *, *, #2509, .F. ) ;
#4112 = CARTESIAN_POINT ( 'NONE',  ( -212.2032458117903104, 73.84851424090838634, 62.50000000000001421 ) ) ;
#4113 = LINE ( 'NONE', #15518, #692 ) ;
#4114 = CARTESIAN_POINT ( 'NONE',  ( -65.00992063630958739, -95.23217577251027421, -44.98760859132558210 ) ) ;
#4115 = ORIENTED_EDGE ( 'NONE', *, *, #1160, .F. ) ;
#4116 = CARTESIAN_POINT ( 'NONE',  ( -92.59262256747321373, 110.5691553257988460, -26.35917033480641436 ) ) ;
#4117 = CYLINDRICAL_SURFACE ( 'NONE', #8541, 10.24900000000000055 ) ;
#4118 = CARTESIAN_POINT ( 'NONE',  ( -62.81538793034061285, 92.72253132893551708, -15.00000000000001421 ) ) ;
#4119 = LINE ( 'NONE', #18051, #9025 ) ;
#4120 = ORIENTED_EDGE ( 'NONE', *, *, #10135, .T. ) ;
#4121 = EDGE_CURVE ( 'NONE', #2855, #3150, #3269, .T. ) ;
#4122 = ADVANCED_FACE ( 'NONE', ( #684 ), #4615, .T. ) ;
#4123 = CARTESIAN_POINT ( 'NONE',  ( -71.24615306438076345, 126.2399288045637462, -167.1454815528550739 ) ) ;
#4124 = EDGE_LOOP ( 'NONE', ( #15387, #18264, #3790, #1957, #16386, #17845 ) ) ;
#4125 = DIRECTION ( 'NONE',  ( 1.000000000000000000, 0.000000000000000000, 0.000000000000000000 ) ) ;
#4126 = LINE ( 'NONE', #9929, #6576 ) ;
#4127 = VERTEX_POINT ( 'NONE', #584 ) ;
#4128 = ORIENTED_EDGE ( 'NONE', *, *, #17270, .T. ) ;
#4129 = EDGE_CURVE ( 'NONE', #2703, #689, #12001, .T. ) ;
#4130 = ADVANCED_FACE ( 'NONE', ( #2173 ), #569, .T. ) ;
#4131 = ORIENTED_EDGE ( 'NONE', *, *, #16690, .F. ) ;
#4132 = DIRECTION ( 'NONE',  ( 0.3420201433256481738, 0.9396926207859158664, -0.000000000000000000 ) ) ;
#4133 = DIRECTION ( 'NONE',  ( 0.3420201433256663814, 0.9396926207859093161, -0.000000000000000000 ) ) ;
#4134 = CARTESIAN_POINT ( 'NONE',  ( -71.24615306438086293, 90.79353891522923448, -167.1454815528550739 ) ) ;
#4135 = ADVANCED_FACE ( 'NONE', ( #13503 ), #13230, .T. ) ;
#4136 = DIRECTION ( 'NONE',  ( -1.000000000000000000, -0.000000000000000000, -0.000000000000000000 ) ) ;
#4137 = LINE ( 'NONE', #2344, #12630 ) ;
#4138 = ORIENTED_EDGE ( 'NONE', *, *, #17597, .T. ) ;
#4139 = EDGE_CURVE ( 'NONE', #7061, #16660, #14904, .T. ) ;
#4140 = CARTESIAN_POINT ( 'NONE',  ( -194.4437806548868934, -111.0842361345572158, 18.23991632971911869 ) ) ;
#4141 = ORIENTED_EDGE ( 'NONE', *, *, #7780, .T. ) ;
#4142 = CARTESIAN_POINT ( 'NONE',  ( -57.08002265617300708, 84.22855780814606419, -15.00000000000001421 ) ) ;
#4143 = EDGE_CURVE ( 'NONE', #6870, #14184, #4781, .T. ) ;
#4144 = ADVANCED_FACE ( 'NONE', ( #10500 ), #16196, .T. ) ;
#4145 = DIRECTION ( 'NONE',  ( 0.000000000000000000, 0.000000000000000000, 1.000000000000000000 ) ) ;
#4146 = VECTOR ( 'NONE', #2176, 1000.000000000000000 ) ;
#4147 = VERTEX_POINT ( 'NONE', #10690 ) ;
#4148 = DIRECTION ( 'NONE',  ( -1.000000000000000000, 0.000000000000000000, 0.000000000000000000 ) ) ;
#4149 = ORIENTED_EDGE ( 'NONE', *, *, #1063, .F. ) ;
#4150 = ADVANCED_FACE ( 'NONE', ( #3572 ), #9113, .T. ) ;
#4151 = ORIENTED_EDGE ( 'NONE', *, *, #8674, .F. ) ;
#4152 = CARTESIAN_POINT ( 'NONE',  ( -64.58002265617299997, 84.22855780814606419, -35.00000000000000000 ) ) ;
#4153 = CIRCLE ( 'NONE', #6834, 11.04359719766050141 ) ;
#4154 = CARTESIAN_POINT ( 'NONE',  ( -71.24615306438111872, 18.53690796522925055, -167.1454815528550739 ) ) ;
#4155 = CARTESIAN_POINT ( 'NONE',  ( -71.24615306438083451, 97.96559495456375544, 15.00000000000006928 ) ) ;
#4156 = ORIENTED_EDGE ( 'NONE', *, *, #3527, .T. ) ;
#4157 = ORIENTED_EDGE ( 'NONE', *, *, #3801, .T. ) ;
#4158 = CARTESIAN_POINT ( 'NONE',  ( -24.58056302216690625, 50.89799459937560755, -26.69769766716196457 ) ) ;
#4159 = CARTESIAN_POINT ( 'NONE',  ( 103.5381772159376084, -111.0842361345572158, 36.00000000000000711 ) ) ;
#4160 = ORIENTED_EDGE ( 'NONE', *, *, #10891, .F. ) ;
#4161 = PLANE ( 'NONE',  #11694 ) ;
#4162 = PLANE ( 'NONE',  #7803 ) ;
#4163 = CARTESIAN_POINT ( 'NONE',  ( -70.27900850916093134, -47.21335801510345220, 15.00000000000008171 ) ) ;
#4164 = ORIENTED_EDGE ( 'NONE', *, *, #930, .T. ) ;
#4165 = DIRECTION ( 'NONE',  ( 0.000000000000000000, 1.000000000000000000, 0.000000000000000000 ) ) ;
#4166 = CARTESIAN_POINT ( 'NONE',  ( -47.13906347517657025, 79.99098546104539764, -15.00000000000001421 ) ) ;
#4167 = ORIENTED_EDGE ( 'NONE', *, *, #2778, .F. ) ;
#4168 = CARTESIAN_POINT ( 'NONE',  ( 5.299999999999998934, 7.505553499465141165, -1.387778780781445676E-14 ) ) ;
#4169 = VERTEX_POINT ( 'NONE', #14707 ) ;
#4170 = VECTOR ( 'NONE', #1464, 1000.000000000000000 ) ;
#4171 = CARTESIAN_POINT ( 'NONE',  ( -81.37409655828237476, -96.08423613455721579, -28.18308811886549847 ) ) ;
#4172 = ORIENTED_EDGE ( 'NONE', *, *, #13629, .T. ) ;
#4173 = CARTESIAN_POINT ( 'NONE',  ( -59.20641439073742873, 73.63336328296978195, -167.1454815528550739 ) ) ;
#4174 = DIRECTION ( 'NONE',  ( -0.9396926207859145341, 0.3420201433256519485, 1.086737899652996918E-16 ) ) ;
#4175 = DIRECTION ( 'NONE',  ( 0.000000000000000000, 0.000000000000000000, 1.000000000000000000 ) ) ;
#4176 = ORIENTED_EDGE ( 'NONE', *, *, #14943, .F. ) ;
#4177 = CARTESIAN_POINT ( 'NONE',  ( -57.08002265617300708, 84.22855780814606419, -47.49999999999999289 ) ) ;
#4178 = LINE ( 'NONE', #14203, #2058 ) ;
#4179 = CARTESIAN_POINT ( 'NONE',  ( -68.99615306438111872, 13.96152643166267993, -167.1454815528550739 ) ) ;
#4180 = CIRCLE ( 'NONE', #5349, 10.24900000000001477 ) ;
#4181 = DIRECTION ( 'NONE',  ( 0.000000000000000000, 0.000000000000000000, -1.000000000000000000 ) ) ;
#4182 = ORIENTED_EDGE ( 'NONE', *, *, #4222, .T. ) ;
#4183 = DIRECTION ( 'NONE',  ( -0.000000000000000000, -1.000000000000000000, 0.000000000000000000 ) ) ;
#4184 = VECTOR ( 'NONE', #1463, 1000.000000000000114 ) ;
#4185 = LINE ( 'NONE', #17418, #16908 ) ;
#4186 = CARTESIAN_POINT ( 'NONE',  ( 0.5805565836007609004, -3.752776749732712691, -6.500000000000033751 ) ) ;
#4187 = PLANE ( 'NONE',  #10809 ) ;
#4188 = VERTEX_POINT ( 'NONE', #7697 ) ;
#4189 = DIRECTION ( 'NONE',  ( 0.000000000000000000, 0.000000000000000000, 1.000000000000000000 ) ) ;
#4190 = LINE ( 'NONE', #8407, #10112 ) ;
#4191 = LINE ( 'NONE', #5678, #1516 ) ;
#4192 = DIRECTION ( 'NONE',  ( -1.000000000000000000, -2.062304371594500740E-16, -0.000000000000000000 ) ) ;
#4193 = ORIENTED_EDGE ( 'NONE', *, *, #6530, .T. ) ;
#4194 = AXIS2_PLACEMENT_3D ( 'NONE', #11882, #13302, #16360 ) ;
#4195 = EDGE_LOOP ( 'NONE', ( #4991, #10816, #5222, #6077 ) ) ;
#4196 = VECTOR ( 'NONE', #13032, 1000.000000000000000 ) ;
#4197 = VECTOR ( 'NONE', #8219, 1000.000000000000000 ) ;
#4199 = EDGE_CURVE ( 'NONE', #17497, #2231, #13407, .T. ) ;
#4198 = DIRECTION ( 'NONE',  ( -5.204170427930409450E-16, 0.000000000000000000, 1.000000000000000000 ) ) ;
#4200 = VERTEX_POINT ( 'NONE', #14617 ) ;
#4201 = CARTESIAN_POINT ( 'NONE',  ( 0.000000000000000000, 0.000000000000000000, 0.000000000000000000 ) ) ;
#4202 = CARTESIAN_POINT ( 'NONE',  ( -107.5926225674731711, 57.88796029049330372, 22.33417033480641223 ) ) ;
#4203 = DIRECTION ( 'NONE',  ( 1.000000000000000000, 0.000000000000000000, 5.204170427930409450E-16 ) ) ;
#4204 = ORIENTED_EDGE ( 'NONE', *, *, #2537, .F. ) ;
#4205 = AXIS2_PLACEMENT_3D ( 'NONE', #4399, #15895, #16940 ) ;
#4206 = CARTESIAN_POINT ( 'NONE',  ( -71.24615306438063556, 135.6647067545637526, 15.00000000000006928 ) ) ;
#4207 = LINE ( 'NONE', #1490, #1948 ) ;
#4208 = LINE ( 'NONE', #1674, #8540 ) ;
#4209 = CARTESIAN_POINT ( 'NONE',  ( -68.99615306438079188, 89.97460588813025595, 15.00000000000006928 ) ) ;
#4210 = VERTEX_POINT ( 'NONE', #13600 ) ;
#4211 = VECTOR ( 'NONE', #12261, 1000.000000000000000 ) ;
#4212 = AXIS2_PLACEMENT_3D ( 'NONE', #4652, #15977, #352 ) ;
#4213 = VECTOR ( 'NONE', #16045, 1000.000000000000114 ) ;
#4214 = CARTESIAN_POINT ( 'NONE',  ( -71.24615306438106188, 38.27533460456375281, 15.00000000000006928 ) ) ;
#4215 = EDGE_LOOP ( 'NONE', ( #17213, #12397, #6703, #14035 ) ) ;
#4216 = LINE ( 'NONE', #2915, #14070 ) ;
#4217 = LINE ( 'NONE', #1681, #16996 ) ;
#4218 = ORIENTED_EDGE ( 'NONE', *, *, #6157, .T. ) ;
#4219 = VERTEX_POINT ( 'NONE', #782 ) ;
#4220 = VECTOR ( 'NONE', #2943, 1000.000000000000000 ) ;
#4221 = ORIENTED_EDGE ( 'NONE', *, *, #12228, .F. ) ;
#4222 = EDGE_CURVE ( 'NONE', #15084, #6521, #1902, .T. ) ;
#4223 = VECTOR ( 'NONE', #18195, 1000.000000000000000 ) ;
#4224 = CARTESIAN_POINT ( 'NONE',  ( -71.24615306438070661, 141.9478920545637664, -167.1454815528550739 ) ) ;
#4225 = CARTESIAN_POINT ( 'NONE',  ( -107.5926225674731853, 110.5691553257988460, 26.35917033480641436 ) ) ;
#4226 = CARTESIAN_POINT ( 'NONE',  ( -71.24615306438109030, 25.70896400456376796, -167.1454815528550739 ) ) ;
#4227 = FACE_OUTER_BOUND ( 'NONE', #5264, .T. ) ;
#4228 = CARTESIAN_POINT ( 'NONE',  ( -36.44155368744861079, 56.74635804676026396, 22.50216374311547440 ) ) ;
#4229 = EDGE_LOOP ( 'NONE', ( #16511, #1531, #15557, #3137, #14602, #4397, #12872, #17375, #14562 ) ) ;
#4230 = ORIENTED_EDGE ( 'NONE', *, *, #5620, .F. ) ;
#4231 = AXIS2_PLACEMENT_3D ( 'NONE', #7587, #4589, #5979 ) ;
#4232 = EDGE_CURVE ( 'NONE', #11248, #7349, #2371, .T. ) ;
#4233 = CARTESIAN_POINT ( 'NONE',  ( -68.99615306438104767, 24.00116023813026089, -15.00000000000001421 ) ) ;
#4234 = PLANE ( 'NONE',  #5681 ) ;
#4235 = EDGE_LOOP ( 'NONE', ( #638, #9998, #9682, #5180 ) ) ;
#4236 = AXIS2_PLACEMENT_3D ( 'NONE', #15652, #14333, #17303 ) ;
#4237 = CARTESIAN_POINT ( 'NONE',  ( -115.4692715616776866, -94.42547395655694231, -5.919112368231730592 ) ) ;
#4238 = VERTEX_POINT ( 'NONE', #7513 ) ;
#4239 = EDGE_CURVE ( 'NONE', #2549, #7660, #408, .T. ) ;
#4240 = ADVANCED_FACE ( 'NONE', ( #3294 ), #7612, .T. ) ;
#4241 = ORIENTED_EDGE ( 'NONE', *, *, #7421, .F. ) ;
#4242 = EDGE_CURVE ( 'NONE', #17405, #6830, #13880, .T. ) ;
#4243 = CIRCLE ( 'NONE', #8736, 180.8515291679561585 ) ;
#4244 = ADVANCED_FACE ( 'NONE', ( #3952 ), #9471, .T. ) ;
#4245 = DIRECTION ( 'NONE',  ( -0.9475106458593564041, -0.3197242186372270534, -0.000000000000000000 ) ) ;
#4246 = CARTESIAN_POINT ( 'NONE',  ( 0.000000000000000000, -91.08423613455721579, -10.65431531532567710 ) ) ;
#4247 = ORIENTED_EDGE ( 'NONE', *, *, #12937, .T. ) ;
#4248 = CONTEXT_DEPENDENT_SHAPE_REPRESENTATION ( #14810, #18209 ) ;
#4249 = VECTOR ( 'NONE', #734, 1000.000000000000000 ) ;
#4250 = ORIENTED_EDGE ( 'NONE', *, *, #3796, .T. ) ;
#4251 = VECTOR ( 'NONE', #18350, 1000.000000000000000 ) ;
#4252 = DIRECTION ( 'NONE',  ( 0.000000000000000000, 0.000000000000000000, -1.000000000000000000 ) ) ;
#4253 = DIRECTION ( 'NONE',  ( 1.000000000000000000, 0.000000000000000000, 3.771137991253934490E-16 ) ) ;
#4254 = VERTEX_POINT ( 'NONE', #6668 ) ;
#4255 = EDGE_CURVE ( 'NONE', #15074, #7696, #10153, .T. ) ;
#4256 = CARTESIAN_POINT ( 'NONE',  ( -107.5926225674731853, 60.58224449241411946, 25.00000000000000000 ) ) ;
#4257 = CARTESIAN_POINT ( 'NONE',  ( -64.09025127992791226, 109.3109350805793270, 37.50000000000000000 ) ) ;
#4258 = ADVANCED_FACE ( 'NONE', ( #2268 ), #13686, .T. ) ;
#4259 = LINE ( 'NONE', #12871, #386 ) ;
#4260 = EDGE_CURVE ( 'NONE', #12660, #505, #8063, .T. ) ;
#4261 = B_SPLINE_CURVE_WITH_KNOTS ( 'NONE', 3,
 ( #8261, #18170, #3666, #16653, #2451, #14975 ),
 .UNSPECIFIED., .F., .F.,
 ( 4, 2, 4 ),
 ( 0.0004789955798651479406, 0.001874570251607515087, 0.003270144923349882233 ),
 .UNSPECIFIED. ) ;
#4262 = VERTEX_POINT ( 'NONE', #3767 ) ;
#4263 = CARTESIAN_POINT ( 'NONE',  ( -67.02098183716937285, 79.99098546104525553, -15.00000000000001421 ) ) ;
#4264 = VERTEX_POINT ( 'NONE', #15167 ) ;
#4265 = VECTOR ( 'NONE', #17151, 1000.000000000000000 ) ;
#4266 = EDGE_CURVE ( 'NONE', #5703, #1230, #8166, .T. ) ;
#4267 = ORIENTED_EDGE ( 'NONE', *, *, #16258, .T. ) ;
#4268 = DIRECTION ( 'NONE',  ( 0.000000000000000000, 0.000000000000000000, 1.000000000000000000 ) ) ;
#4269 = AXIS2_PLACEMENT_3D ( 'NONE', #4082, #12700, #18399 ) ;
#4270 = ORIENTED_EDGE ( 'NONE', *, *, #8011, .T. ) ;
#4271 = EDGE_CURVE ( 'NONE', #827, #5082, #2647, .T. ) ;
#4272 = EDGE_LOOP ( 'NONE', ( #17189, #3627, #9483, #13001 ) ) ;
#4273 = ADVANCED_FACE ( 'NONE', ( #15268 ), #11648, .T. ) ;
#4274 = DIRECTION ( 'NONE',  ( 0.3420201433256481738, -0.9396926207859158664, 0.000000000000000000 ) ) ;
#4275 = VECTOR ( 'NONE', #13637, 1000.000000000000000 ) ;
#4276 = ORIENTED_EDGE ( 'NONE', *, *, #10870, .F. ) ;
#4277 = DIRECTION ( 'NONE',  ( 0.000000000000000000, 0.000000000000000000, -1.000000000000000000 ) ) ;
#4278 = PLANE ( 'NONE',  #1469 ) ;
#4279 = PLANE ( 'NONE',  #17353 ) ;
#4280 = DIRECTION ( 'NONE',  ( 0.000000000000000000, 0.000000000000000000, 1.000000000000000000 ) ) ;
#4281 = VERTEX_POINT ( 'NONE', #12288 ) ;
#4282 = CARTESIAN_POINT ( 'NONE',  ( -60.06546592763139358, -91.08423613455721579, 28.18308811886542742 ) ) ;
#4283 = AXIS2_PLACEMENT_3D ( 'NONE', #11034, #16719, #5411 ) ;
#4284 = VECTOR ( 'NONE', #9422, 1000.000000000000000 ) ;
#4285 = EDGE_CURVE ( 'NONE', #16809, #16358, #5344, .T. ) ;
#4286 = CARTESIAN_POINT ( 'NONE',  ( -70.71978124295696944, -96.08423613455721579, 5.204170427930421283E-15 ) ) ;
#4287 = CARTESIAN_POINT ( 'NONE',  ( -3.386515864108431195, 32.64046595754329161, 37.63508979505212437 ) ) ;
#4288 = VERTEX_POINT ( 'NONE', #8351 ) ;
#4289 = DIRECTION ( 'NONE',  ( 0.000000000000000000, 0.000000000000000000, -1.000000000000000000 ) ) ;
#4290 = LINE ( 'NONE', #2610, #6906 ) ;
#4291 = VECTOR ( 'NONE', #2881, 1000.000000000000000 ) ;
#4292 = CYLINDRICAL_SURFACE ( 'NONE', #15254, 42.49926016645017057 ) ;
#4293 = CARTESIAN_POINT ( 'NONE',  ( -57.08002265617300708, 84.22855780814606419, 15.00000000000006928 ) ) ;
#4294 = ORIENTED_EDGE ( 'NONE', *, *, #12082, .T. ) ;
#4295 = ORIENTED_EDGE ( 'NONE', *, *, #8314, .T. ) ;
#4296 = AXIS2_PLACEMENT_3D ( 'NONE', #5778, #8682, #13088 ) ;
#4297 = DIRECTION ( 'NONE',  ( 1.000000000000000000, 0.000000000000000000, 5.077734830647299712E-16 ) ) ;
#4298 = VERTEX_POINT ( 'NONE', #6851 ) ;
#4299 = CARTESIAN_POINT ( 'NONE',  ( -68.12361985383350316, 84.22855780814606419, -35.00000000000000000 ) ) ;
#4300 = VERTEX_POINT ( 'NONE', #5167 ) ;
#4301 = CARTESIAN_POINT ( 'NONE',  ( -123.4618227840623632, -151.5628872026273086, 57.00000000000000000 ) ) ;
#4302 = CARTESIAN_POINT ( 'NONE',  ( -68.99615306438077766, 114.4924912316626688, -15.00000000000001421 ) ) ;
#4303 = LINE ( 'NONE', #2817, #1565 ) ;
#4304 = EDGE_LOOP ( 'NONE', ( #3023, #8778, #14360, #14095 ) ) ;
#4305 = DIRECTION ( 'NONE',  ( 1.000000000000000000, -0.000000000000000000, -0.000000000000000000 ) ) ;
#4306 = VECTOR ( 'NONE', #10242, 1000.000000000000000 ) ;
#4307 = VECTOR ( 'NONE', #15014, 1000.000000000000114 ) ;
#4308 = DIRECTION ( 'NONE',  ( 0.9396926207859097602, 0.3420201433256649937, 0.000000000000000000 ) ) ;
#4309 = ORIENTED_EDGE ( 'NONE', *, *, #250, .T. ) ;
#4310 = EDGE_CURVE ( 'NONE', #15152, #15440, #969, .T. ) ;
#4311 = CARTESIAN_POINT ( 'NONE',  ( -68.99615306438087714, 52.27549408813020904, 15.00000000000006928 ) ) ;
#4312 = ORIENTED_EDGE ( 'NONE', *, *, #6375, .F. ) ;
#4313 = ORIENTED_EDGE ( 'NONE', *, *, #4027, .F. ) ;
#4314 = AXIS2_PLACEMENT_3D ( 'NONE', #2781, #9700, #2875 ) ;
#4315 = EDGE_CURVE ( 'NONE', #13617, #4782, #4064, .T. ) ;
#4316 = VECTOR ( 'NONE', #4087, 1000.000000000000000 ) ;
#4317 = AXIS2_PLACEMENT_3D ( 'NONE', #625, #4727, #13091 ) ;
#4318 = LINE ( 'NONE', #12935, #4614 ) ;
#4319 = CARTESIAN_POINT ( 'NONE',  ( 0.06682554136344981410, -4.993536075455556222, 4.350941807883138779 ) ) ;
#4320 = LINE ( 'NONE', #4580, #1183 ) ;
#4321 = CARTESIAN_POINT ( 'NONE',  ( -68.99615306438091977, 76.79337943166271430, -167.1454815528550739 ) ) ;
#4322 = CYLINDRICAL_SURFACE ( 'NONE', #11999, 11.04359719766050141 ) ;
#4323 = ORIENTED_EDGE ( 'NONE', *, *, #1601, .T. ) ;
#4324 = VECTOR ( 'NONE', #10321, 1000.000000000000000 ) ;
#4325 = DIRECTION ( 'NONE',  ( -1.000000000000000000, 0.000000000000000000, 0.000000000000000000 ) ) ;
#4326 = ORIENTED_EDGE ( 'NONE', *, *, #13063, .T. ) ;
#4327 = DIRECTION ( 'NONE',  ( 0.9396926207859084279, 0.3420201433256686574, 4.890320548438448905E-16 ) ) ;
#4328 = DIRECTION ( 'NONE',  ( -1.000000000000000000, 1.558623840612994987E-16, 0.000000000000000000 ) ) ;
#4329 = ORIENTED_EDGE ( 'NONE', *, *, #5149, .F. ) ;
#4330 = AXIS2_PLACEMENT_3D ( 'NONE', #611, #9041, #2106 ) ;
#4331 = AXIS2_PLACEMENT_3D ( 'NONE', #9404, #17716, #6480 ) ;
#4332 = CYLINDRICAL_SURFACE ( 'NONE', #15784, 7.168074330098680669 ) ;
#4334 = ORIENTED_EDGE ( 'NONE', *, *, #11316, .T. ) ;
#4333 = AXIS2_PLACEMENT_3D ( 'NONE', #16070, #13106, #3181 ) ;
#4335 = EDGE_CURVE ( 'NONE', #14981, #2271, #12484, .T. ) ;
#4336 = ORIENTED_EDGE ( 'NONE', *, *, #8337, .F. ) ;
#4337 = EDGE_CURVE ( 'NONE', #4498, #4736, #11169, .T. ) ;
#4338 = CYLINDRICAL_SURFACE ( 'NONE', #2831, 12.50000000000000355 ) ;
#4339 = DIRECTION ( 'NONE',  ( -0.9396926207859158664, 0.3420201433256481738, 1.086737899652998397E-16 ) ) ;
#4340 = VECTOR ( 'NONE', #3193, 1000.000000000000000 ) ;
#4341 = EDGE_LOOP ( 'NONE', ( #16627, #4710, #5829, #2244 ) ) ;
#4342 = VECTOR ( 'NONE', #10748, 1000.000000000000000 ) ;
#4343 = CIRCLE ( 'NONE', #16877, 6.500000000000039968 ) ;
#4344 = LINE ( 'NONE', #16879, #9401 ) ;
#4345 = EDGE_LOOP ( 'NONE', ( #5198, #13413, #15897, #2355 ) ) ;
#4346 = DIRECTION ( 'NONE',  ( -1.000000000000000000, -2.062304371594500494E-16, -0.000000000000000000 ) ) ;
#4347 = DIRECTION ( 'NONE',  ( 0.000000000000000000, 0.000000000000000000, 1.000000000000000000 ) ) ;
#4348 = CARTESIAN_POINT ( 'NONE',  ( -71.24615306438114715, 15.39531531522927921, -167.1454815528550739 ) ) ;
#4349 = ORIENTED_EDGE ( 'NONE', *, *, #7237, .F. ) ;
#4350 = EDGE_CURVE ( 'NONE', #6267, #17849, #16714, .T. ) ;
#4351 = LINE ( 'NONE', #13134, #14621 ) ;
#4352 = VERTEX_POINT ( 'NONE', #14062 ) ;
#4353 = EDGE_CURVE ( 'NONE', #14012, #8703, #6952, .T. ) ;
#4354 = VERTEX_POINT ( 'NONE', #16482 ) ;
#4355 = LINE ( 'NONE', #10064, #9697 ) ;
#4356 = TOROIDAL_SURFACE ( 'NONE', #10326, 2.168074330098679336, 5.000000000000000000 ) ;
#4357 = CIRCLE ( 'NONE', #15992, 4.599999999999999645 ) ;
#4358 = EDGE_LOOP ( 'NONE', ( #3277, #7882, #8516, #12796 ) ) ;
#4359 = EDGE_CURVE ( 'NONE', #12641, #14842, #3671, .T. ) ;
#4360 = EDGE_CURVE ( 'NONE', #14903, #848, #11054, .T. ) ;
#4361 = EDGE_CURVE ( 'NONE', #11131, #12093, #13040, .T. ) ;
#4362 = FACE_OUTER_BOUND ( 'NONE', #4813, .T. ) ;
#4363 = FACE_OUTER_BOUND ( 'NONE', #17420, .T. ) ;
#4364 = CARTESIAN_POINT ( 'NONE',  ( -71.24615306438109030, 31.10327856522923540, 15.00000000000006928 ) ) ;
#4365 = ORIENTED_EDGE ( 'NONE', *, *, #9270, .F. ) ;
#4366 = FACE_OUTER_BOUND ( 'NONE', #18110, .T. ) ;
#4367 = CARTESIAN_POINT ( 'NONE',  ( -71.24615306438086293, 100.2183168652291982, -15.00000000000001421 ) ) ;
#4368 = DIRECTION ( 'NONE',  ( 0.000000000000000000, 0.000000000000000000, -1.000000000000000000 ) ) ;
#4369 = DIRECTION ( 'NONE',  ( -0.9396926207859084279, 0.3420201433256686574, -4.890320548438448905E-16 ) ) ;
#4370 = ORIENTED_EDGE ( 'NONE', *, *, #8838, .F. ) ;
#4371 = ADVANCED_FACE ( 'NONE', ( #7058 ), #4234, .T. ) ;
#4372 = DIRECTION ( 'NONE',  ( 0.000000000000000000, 0.000000000000000000, 1.000000000000000000 ) ) ;
#4373 = CARTESIAN_POINT ( 'NONE',  ( -71.24615306438080609, 109.6430948152292189, 15.00000000000006928 ) ) ;
#4374 = CARTESIAN_POINT ( 'NONE',  ( -68.99615306438111872, 20.24471173166267235, -167.1454815528550739 ) ) ;
#4375 = VERTEX_POINT ( 'NONE', #12853 ) ;
#4376 = EDGE_CURVE ( 'NONE', #8935, #9204, #7, .T. ) ;
#4377 = DIRECTION ( 'NONE',  ( 1.000000000000000000, 0.000000000000000000, 3.771137991253928573E-16 ) ) ;
#4378 = EDGE_CURVE ( 'NONE', #4994, #18486, #8555, .T. ) ;
#4379 = LINE ( 'NONE', #15964, #6282 ) ;
#4380 = CARTESIAN_POINT ( 'NONE',  ( -45.21333244822126574, 88.15687341518456321, -15.00000000000001421 ) ) ;
#4381 = ORIENTED_EDGE ( 'NONE', *, *, #14548, .T. ) ;
#4382 = ORIENTED_EDGE ( 'NONE', *, *, #5830, .F. ) ;
#4383 = EDGE_CURVE ( 'NONE', #15468, #4644, #6244, .T. ) ;
#4384 = DIRECTION ( 'NONE',  ( 0.000000000000000000, 0.000000000000000000, 1.000000000000000000 ) ) ;
#4385 = DIRECTION ( 'NONE',  ( 0.000000000000000000, 0.000000000000000000, 1.000000000000000000 ) ) ;
#4386 = SHAPE_REPRESENTATION_RELATIONSHIP ( 'NONE' , 'NONE' ,  #16862, #14171 ) ;
#4387 = LINE ( 'NONE', #10095, #2800 ) ;
#4388 = LINE ( 'NONE', #1487, #4009 ) ;
#4389 = VERTEX_POINT ( 'NONE', #1695 ) ;
#4390 = DIRECTION ( 'NONE',  ( 0.3197242186372270534, 0.9475106458593564041, 0.000000000000000000 ) ) ;
#4391 = DIRECTION ( 'NONE',  ( 1.156482317317869999E-16, 0.000000000000000000, 1.000000000000000000 ) ) ;
#4392 = SURFACE_SIDE_STYLE ('',( #14236 ) ) ;
#4393 = CARTESIAN_POINT ( 'NONE',  ( -94.45685920050698314, -47.21335801510345220, -15.00000000000001421 ) ) ;
#4394 = ORIENTED_EDGE ( 'NONE', *, *, #18323, .F. ) ;
#4395 = DIRECTION ( 'NONE',  ( 1.000000000000000000, 1.119176436114069332E-16, 0.000000000000000000 ) ) ;
#4396 = CARTESIAN_POINT ( 'NONE',  ( -71.24615306438117557, 3.717815454563750954, -15.00000000000001421 ) ) ;
#4397 = ORIENTED_EDGE ( 'NONE', *, *, #1407, .F. ) ;
#4398 = CARTESIAN_POINT ( 'NONE',  ( -68.12361985383350316, 84.22855780814606419, 68.73600986863397111 ) ) ;
#4399 = CARTESIAN_POINT ( 'NONE',  ( -57.89103256796045116, 73.45256821284057480, -15.00000000000001421 ) ) ;
#4400 = VERTEX_POINT ( 'NONE', #8819 ) ;
#4401 = ORIENTED_EDGE ( 'NONE', *, *, #1290, .F. ) ;
#4402 = CARTESIAN_POINT ( 'NONE',  ( -68.99615306438089135, 86.83301323813024908, 15.00000000000006928 ) ) ;
#4403 = CARTESIAN_POINT ( 'NONE',  ( -71.24615306438076345, 119.0678727652292253, 15.00000000000006928 ) ) ;
#4404 = LINE ( 'NONE', #2834, #14606 ) ;
#4405 = CARTESIAN_POINT ( 'NONE',  ( -68.99615306438116136, 2.010011688130275420, -15.00000000000001421 ) ) ;
#4406 = DIRECTION ( 'NONE',  ( -0.000000000000000000, -0.000000000000000000, 1.000000000000000000 ) ) ;
#4407 = ORIENTED_EDGE ( 'NONE', *, *, #3679, .T. ) ;
#4408 = CARTESIAN_POINT ( 'NONE',  ( -68.99615306438109030, 17.71797493813028268, 15.00000000000006928 ) ) ;
#4410 = EDGE_CURVE ( 'NONE', #18251, #2177, #12678, .T. ) ;
#4409 = ORIENTED_EDGE ( 'NONE', *, *, #2293, .F. ) ;
#4411 = DIRECTION ( 'NONE',  ( 0.9396926207859084279, 0.3420201433256686574, 4.890320548438448905E-16 ) ) ;
#4412 = CARTESIAN_POINT ( 'NONE',  ( -44.89980253466632831, 81.41924511788819530, -167.1454815528550739 ) ) ;
#4413 = ORIENTED_EDGE ( 'NONE', *, *, #5009, .F. ) ;
#4414 = CARTESIAN_POINT ( 'NONE',  ( -59.37303238940180705, 94.21775734381046163, 15.00000000000006928 ) ) ;
#4415 = ORIENTED_EDGE ( 'NONE', *, *, #8830, .F. ) ;
#4416 = ORIENTED_EDGE ( 'NONE', *, *, #9855, .F. ) ;
#4417 = CARTESIAN_POINT ( 'NONE',  ( -71.24615306438086293, 100.2183168652291982, 15.00000000000006928 ) ) ;
#4418 = CARTESIAN_POINT ( 'NONE',  ( -71.24615306438080609, 109.6430948152292189, -167.1454815528550739 ) ) ;
#4419 = CARTESIAN_POINT ( 'NONE',  ( -71.24615306438076345, 131.6342433652292243, 15.00000000000006928 ) ) ;
#4420 = ORIENTED_EDGE ( 'NONE', *, *, #4595, .F. ) ;
#4421 = CARTESIAN_POINT ( 'NONE',  ( -25.66933353722516031, -95.65021616327642562, 5.654315315325686875 ) ) ;
#4422 = VERTEX_POINT ( 'NONE', #2928 ) ;
#4423 = AXIS2_PLACEMENT_3D ( 'NONE', #11226, #6905, #12633 ) ;
#4424 = DIRECTION ( 'NONE',  ( 0.000000000000000000, 0.000000000000000000, -1.000000000000000000 ) ) ;
#4425 = DIRECTION ( 'NONE',  ( -0.9396926207859069846, 0.3420201433256723766, 1.086737899652988166E-16 ) ) ;
#4426 = CARTESIAN_POINT ( 'NONE',  ( -67.12361985383350316, 84.22855780814606419, -62.50000000000000000 ) ) ;
#4427 = ORIENTED_EDGE ( 'NONE', *, *, #17272, .T. ) ;
#4428 = CARTESIAN_POINT ( 'NONE',  ( 0.000000000000000000, 0.000000000000000000, 0.000000000000000000 ) ) ;
#4429 = EDGE_LOOP ( 'NONE', ( #18514, #18372, #3255, #18470 ) ) ;
#4430 = EDGE_CURVE ( 'NONE', #15988, #6870, #14339, .T. ) ;
#4431 = ORIENTED_EDGE ( 'NONE', *, *, #9865, .F. ) ;
#4432 = AXIS2_PLACEMENT_3D ( 'NONE', #8905, #1884, #390 ) ;
#4433 = ORIENTED_EDGE ( 'NONE', *, *, #16777, .T. ) ;
#4434 = CARTESIAN_POINT ( 'NONE',  ( -71.24615306438086293, 90.79353891522923448, -15.00000000000001421 ) ) ;
#4435 = ADVANCED_FACE ( 'NONE', ( #14519 ), #14256, .F. ) ;
#4436 = DIRECTION ( 'NONE',  ( 0.000000000000000000, 0.000000000000000000, 1.000000000000000000 ) ) ;
#4437 = CARTESIAN_POINT ( 'NONE',  ( -102.5926225674731569, 65.58224449241410525, -20.00000000000000355 ) ) ;
#4438 = ORIENTED_EDGE ( 'NONE', *, *, #7306, .F. ) ;
#4439 = DIRECTION ( 'NONE',  ( 1.000000000000000000, 0.000000000000000000, 0.000000000000000000 ) ) ;
#4440 = CARTESIAN_POINT ( 'NONE',  ( -97.59262256747321373, 117.8748711238780515, -25.00000000000000000 ) ) ;
#4441 = DIRECTION ( 'NONE',  ( 0.000000000000000000, 0.000000000000000000, 1.000000000000000000 ) ) ;
#4442 = DIRECTION ( 'NONE',  ( 0.000000000000000000, 1.000000000000000000, 0.000000000000000000 ) ) ;
#4443 = ORIENTED_EDGE ( 'NONE', *, *, #14538, .F. ) ;
#4444 = CARTESIAN_POINT ( 'NONE',  ( -57.08002265617300708, 84.22855780814606419, -15.00000000000001421 ) ) ;
#4445 = VECTOR ( 'NONE', #7169, 1000.000000000000000 ) ;
#4446 = CARTESIAN_POINT ( 'NONE',  ( -71.24615306438093398, 50.84170520456373765, 15.00000000000006928 ) ) ;
#4447 = DIRECTION ( 'NONE',  ( 7.442644330182800165E-16, -1.000000000000000000, 0.000000000000000000 ) ) ;
#4448 = ORIENTED_EDGE ( 'NONE', *, *, #8615, .T. ) ;
#4449 = EDGE_CURVE ( 'NONE', #864, #1101, #2381, .T. ) ;
#4450 = EDGE_CURVE ( 'NONE', #5525, #15948, #17309, .T. ) ;
#4451 = DIRECTION ( 'NONE',  ( 0.000000000000000000, 0.000000000000000000, 1.000000000000000000 ) ) ;
#4452 = EDGE_CURVE ( 'NONE', #6195, #11833, #1610, .T. ) ;
#4453 = CARTESIAN_POINT ( 'NONE',  ( 0.5805565836007609004, 3.752776749732435135, 6.499999999999981348 ) ) ;
#4454 = ORIENTED_EDGE ( 'NONE', *, *, #17262, .T. ) ;
#4455 = ORIENTED_EDGE ( 'NONE', *, *, #17733, .T. ) ;
#4456 = EDGE_CURVE ( 'NONE', #2929, #8972, #14354, .T. ) ;
#4458 = EDGE_CURVE ( 'NONE', #18474, #4238, #15917, .T. ) ;
#4457 = AXIS2_PLACEMENT_3D ( 'NONE', #3487, #14892, #12105 ) ;
#4459 = CARTESIAN_POINT ( 'NONE',  ( -68.99615306438111872, 8.293196988130274505, 15.00000000000006928 ) ) ;
#4460 = ADVANCED_FACE ( 'NONE', ( #12770 ), #17140, .F. ) ;
#4461 = AXIS2_PLACEMENT_3D ( 'NONE', #6842, #2557, #7132 ) ;
#4462 =( LENGTH_UNIT ( ) NAMED_UNIT ( * ) SI_UNIT ( .MILLI., .METRE. ) );
#4463 = CARTESIAN_POINT ( 'NONE',  ( -49.75809927370887920, 76.28065702765852052, -15.00000000000001421 ) ) ;
#4464 = ADVANCED_FACE ( 'NONE', ( #5814 ), #15550, .T. ) ;
#4465 = PLANE ( 'NONE',  #11487 ) ;
#4466 = VERTEX_POINT ( 'NONE', #10043 ) ;
#4467 = CARTESIAN_POINT ( 'NONE',  ( -68.99615306438094819, 70.51019413166270056, 15.00000000000006928 ) ) ;
#4468 = CARTESIAN_POINT ( 'NONE',  ( -71.24615306438111872, 21.67850061522927518, -167.1454815528550739 ) ) ;
#4469 = CYLINDRICAL_SURFACE ( 'NONE', #16575, 6.500000000000039968 ) ;
#4470 = DIRECTION ( 'NONE',  ( -5.204170427930409450E-16, 0.000000000000000000, 1.000000000000000000 ) ) ;
#4471 = ORIENTED_EDGE ( 'NONE', *, *, #11817, .F. ) ;
#4472 = CARTESIAN_POINT ( 'NONE',  ( -37.32695181192723766, 91.48526692943180194, 64.45748773249914620 ) ) ;
#4473 = EDGE_CURVE ( 'NONE', #10126, #14988, #15746, .T. ) ;
#4474 = EDGE_CURVE ( 'NONE', #15130, #13519, #11974, .T. ) ;
#4475 = CARTESIAN_POINT ( 'NONE',  ( -57.08002265617300708, 84.22855780814606419, -124.8487082408420861 ) ) ;
#4476 = AXIS2_PLACEMENT_3D ( 'NONE', #7321, #17043, #14159 ) ;
#4477 = ORIENTED_EDGE ( 'NONE', *, *, #10156, .F. ) ;
#4478 = B_SPLINE_CURVE_WITH_KNOTS ( 'NONE', 3,
 ( #15994, #17299, #5887, #10378, #8892, #14587 ),
 .UNSPECIFIED., .F., .F.,
 ( 4, 2, 4 ),
 ( 2.380733003268861808E-07, 0.001898835937927363139, 0.003797433802554399471 ),
 .UNSPECIFIED. ) ;
#4479 = PLANE ( 'NONE',  #9567 ) ;
#4480 = VECTOR ( 'NONE', #5577, 1000.000000000000000 ) ;
#4481 = DIRECTION ( 'NONE',  ( 1.000000000000000000, 0.000000000000000000, 5.077734830647295768E-16 ) ) ;
#4482 = VERTEX_POINT ( 'NONE', #481 ) ;
#4483 = VERTEX_POINT ( 'NONE', #10390 ) ;
#4484 = ORIENTED_EDGE ( 'NONE', *, *, #6284, .F. ) ;
#4485 = CARTESIAN_POINT ( 'NONE',  ( -212.2032458117903104, 84.22855780814606419, 62.50000000000001421 ) ) ;
#4486 = LINE ( 'NONE', #17389, #7548 ) ;
#4487 = AXIS2_PLACEMENT_3D ( 'NONE', #13276, #456, #17555 ) ;
#4488 = ADVANCED_FACE ( 'NONE', ( #4959 ), #14866, .T. ) ;
#4489 = DIRECTION ( 'NONE',  ( 0.000000000000000000, 1.000000000000000000, 0.000000000000000000 ) ) ;
#4490 = CARTESIAN_POINT ( 'NONE',  ( -38.09490121289055509, 73.26749283227019305, 92.50000000000000000 ) ) ;
#4491 = AXIS2_PLACEMENT_3D ( 'NONE', #14233, #11140, #2622 ) ;
#4492 = CARTESIAN_POINT ( 'NONE',  ( 5.233202738124664855, -19.34983604512935074, 57.00000000000000000 ) ) ;
#4493 = AXIS2_PLACEMENT_3D ( 'NONE', #13454, #13552, #8019 ) ;
#4494 = ORIENTED_EDGE ( 'NONE', *, *, #2421, .T. ) ;
#4495 = LINE ( 'NONE', #9179, #1828 ) ;
#4496 = CARTESIAN_POINT ( 'NONE',  ( -71.24615306438111872, 19.42577870456376132, -167.1454815528550739 ) ) ;
#4497 = DIRECTION ( 'NONE',  ( 0.000000000000000000, 0.000000000000000000, 1.000000000000000000 ) ) ;
#4498 = VERTEX_POINT ( 'NONE', #14781 ) ;
#4499 = TOROIDAL_SURFACE ( 'NONE', #2712, 10.65431531532567888, 5.000000000000000000 ) ;
#4500 = PLANE ( 'NONE',  #13024 ) ;
#4501 = CARTESIAN_POINT ( 'NONE',  ( -57.08002265617300708, 84.22855780814606419, -167.1454815528550739 ) ) ;
#4502 = ORIENTED_EDGE ( 'NONE', *, *, #6181, .F. ) ;
#4503 = AXIS2_PLACEMENT_3D ( 'NONE', #10338, #3215, #16813 ) ;
#4504 = VECTOR ( 'NONE', #17919, 1000.000000000000000 ) ;
#4505 = VERTEX_POINT ( 'NONE', #16080 ) ;
#4506 = DIRECTION ( 'NONE',  ( 0.000000000000000000, 0.000000000000000000, -1.000000000000000000 ) ) ;
#4507 = B_SPLINE_CURVE_WITH_KNOTS ( 'NONE', 3,
 ( #12351, #9627, #927, #11238, #1029, #4018 ),
 .UNSPECIFIED., .F., .F.,
 ( 4, 2, 4 ),
 ( 0.0002781749886595805371, 0.001673372216920096913, 0.003068569445180613017 ),
 .UNSPECIFIED. ) ;
#4508 = FACE_OUTER_BOUND ( 'NONE', #14765, .T. ) ;
#4509 = DIRECTION ( 'NONE',  ( -0.000000000000000000, -1.000000000000000000, -0.000000000000000000 ) ) ;
#4510 = EDGE_LOOP ( 'NONE', ( #10998, #14670, #13034, #13949 ) ) ;
#4511 = CARTESIAN_POINT ( 'NONE',  ( -28.46967348631369177, -91.80659809767261947, 8.049312157728774508 ) ) ;
#4512 = ORIENTED_EDGE ( 'NONE', *, *, #16946, .T. ) ;
#4513 = CARTESIAN_POINT ( 'NONE',  ( -71.24615306438096241, 41.41692725456380941, 15.00000000000006928 ) ) ;
#4514 = DIRECTION ( 'NONE',  ( 1.156482317317869999E-16, 0.000000000000000000, 1.000000000000000000 ) ) ;
#4515 = LINE ( 'NONE', #10230, #10042 ) ;
#4516 = DIRECTION ( 'NONE',  ( -0.9396926207859022107, 0.3420201433256853663, -4.890320548438416365E-16 ) ) ;
#4517 = CIRCLE ( 'NONE', #11982, 10.24900000000000055 ) ;
#4518 = VERTEX_POINT ( 'NONE', #16005 ) ;
#4519 = LINE ( 'NONE', #10060, #6549 ) ;
#4520 = VERTEX_POINT ( 'NONE', #14685 ) ;
#4521 = ORIENTED_EDGE ( 'NONE', *, *, #9593, .F. ) ;
#4522 = ADVANCED_FACE ( 'NONE', ( #9181 ), #1881, .T. ) ;
#4523 = VECTOR ( 'NONE', #9659, 1000.000000000000000 ) ;
#4524 = VECTOR ( 'NONE', #16570, 1000.000000000000000 ) ;
#4525 = AXIS2_PLACEMENT_3D ( 'NONE', #2077, #12279, #2261 ) ;
#4526 = DIRECTION ( 'NONE',  ( -2.062304371594500494E-16, 1.000000000000000000, -0.000000000000000000 ) ) ;
#4527 = ORIENTED_EDGE ( 'NONE', *, *, #18318, .F. ) ;
#4528 = CARTESIAN_POINT ( 'NONE',  ( -50.24148097183213935, 76.59466308582166505, -167.1454815528550739 ) ) ;
#4529 = PLANE ( 'NONE',  #2675 ) ;
#4530 = CARTESIAN_POINT ( 'NONE',  ( -70.71978124295668522, -91.08423613455721579, -28.18308811886538479 ) ) ;
#4531 = CARTESIAN_POINT ( 'NONE',  ( 0.2565376335216263959, -2.516992571280132651, 6.499999999999984013 ) ) ;
#4532 = ORIENTED_EDGE ( 'NONE', *, *, #4255, .T. ) ;
#4533 = VECTOR ( 'NONE', #596, 999.9999999999998863 ) ;
#4534 = CARTESIAN_POINT ( 'NONE',  ( -71.24615306438097662, 56.23601976522923707, -15.00000000000001421 ) ) ;
#4535 = DIRECTION ( 'NONE',  ( 0.9396926207859102043, 0.3420201433256637169, 4.890320548438457780E-16 ) ) ;
#4536 = CARTESIAN_POINT ( 'NONE',  ( -68.99615306438089135, 79.93497208166267853, 15.00000000000006928 ) ) ;
#4537 = ORIENTED_EDGE ( 'NONE', *, *, #3771, .T. ) ;
#4538 = CIRCLE ( 'NONE', #1849, 34.36884788726141693 ) ;
#4539 = VECTOR ( 'NONE', #8791, 1000.000000000000000 ) ;
#4540 = DIRECTION ( 'NONE',  ( 1.000000000000000000, 0.000000000000000000, 0.000000000000000000 ) ) ;
#4541 = ADVANCED_FACE ( 'NONE', ( #3547 ), #3365, .T. ) ;
#4542 = CARTESIAN_POINT ( 'NONE',  ( -68.99615306438093398, 52.27549408813023035, -15.00000000000001421 ) ) ;
#4543 = VERTEX_POINT ( 'NONE', #17401 ) ;
#4544 = ORIENTED_EDGE ( 'NONE', *, *, #17224, .T. ) ;
#4545 = TOROIDAL_SURFACE ( 'NONE', #2462, 2.168074330099288183, 5.000000000000000000 ) ;
#4546 = ORIENTED_EDGE ( 'NONE', *, *, #9609, .F. ) ;
#4547 = PLANE ( 'NONE',  #4296 ) ;
#4548 = EDGE_CURVE ( 'NONE', #14915, #12020, #7761, .T. ) ;
#4549 = VECTOR ( 'NONE', #6656, 1000.000000000000000 ) ;
#4550 = AXIS2_PLACEMENT_3D ( 'NONE', #9685, #9781, #7074 ) ;
#4551 = CARTESIAN_POINT ( 'NONE',  ( -115.4052441654534249, 57.88796029049329661, -26.35917033480640015 ) ) ;
#4552 = CARTESIAN_POINT ( 'NONE',  ( -70.06856178257687873, 57.88796029049330372, -22.35917033480642502 ) ) ;
#4553 = DIRECTION ( 'NONE',  ( 0.000000000000000000, 0.000000000000000000, 1.000000000000000000 ) ) ;
#4554 = DIRECTION ( 'NONE',  ( -1.000000000000000000, -5.551115123125786646E-15, 1.387778780781446662E-16 ) ) ;
#4555 = ORIENTED_EDGE ( 'NONE', *, *, #5293, .T. ) ;
#4556 = CARTESIAN_POINT ( 'NONE',  ( -68.99615306438120399, -1.131580961869733448, 15.00000000000006928 ) ) ;
#4557 = DIRECTION ( 'NONE',  ( 1.000000000000000000, 0.000000000000000000, 0.000000000000000000 ) ) ;
#4558 = DIRECTION ( 'NONE',  ( 0.000000000000000000, 0.000000000000000000, -1.000000000000000000 ) ) ;
#4559 = DIRECTION ( 'NONE',  ( -0.000000000000000000, 1.000000000000000000, -0.000000000000000000 ) ) ;
#4560 = CARTESIAN_POINT ( 'NONE',  ( -37.39954651359116866, 91.67990741037236546, 61.51369636248775663 ) ) ;
#4561 = VECTOR ( 'NONE', #16090, 1000.000000000000000 ) ;
#4562 = EDGE_CURVE ( 'NONE', #18509, #14448, #18232, .T. ) ;
#4563 = PLANE ( 'NONE',  #11662 ) ;
#4564 = ADVANCED_FACE ( 'NONE', ( #10309 ), #13381, .T. ) ;
#4565 = ORIENTED_EDGE ( 'NONE', *, *, #9858, .T. ) ;
#4566 = EDGE_CURVE ( 'NONE', #18179, #16605, #8995, .T. ) ;
#4567 = AXIS2_PLACEMENT_3D ( 'NONE', #7023, #13842, #1030 ) ;
#4568 = CARTESIAN_POINT ( 'NONE',  ( -66.00585202009860097, 58.06035137085946474, 25.00000000000000000 ) ) ;
#4569 = VECTOR ( 'NONE', #2455, 1000.000000000000000 ) ;
#4570 = DIRECTION ( 'NONE',  ( 0.000000000000000000, 1.000000000000000000, -0.000000000000000000 ) ) ;
#4571 = ORIENTED_EDGE ( 'NONE', *, *, #9838, .F. ) ;
#4572 = VECTOR ( 'NONE', #1746, 1000.000000000000000 ) ;
#4573 = VERTEX_POINT ( 'NONE', #11806 ) ;
#4574 = EDGE_CURVE ( 'NONE', #8464, #6521, #12079, .T. ) ;
#4575 = VERTEX_POINT ( 'NONE', #10579 ) ;
#4576 = EDGE_CURVE ( 'NONE', #17297, #11154, #17496, .T. ) ;
#4577 = EDGE_CURVE ( 'NONE', #10506, #2278, #13207, .T. ) ;
#4578 = LINE ( 'NONE', #1508, #17754 ) ;
#4579 = LINE ( 'NONE', #277, #18337 ) ;
#4580 = CARTESIAN_POINT ( 'NONE',  ( -71.24615306438069240, 132.5231141045637742, 15.00000000000006928 ) ) ;
#4581 = DIRECTION ( 'NONE',  ( 0.000000000000000000, 1.000000000000000000, 0.000000000000000000 ) ) ;
#4582 = EDGE_CURVE ( 'NONE', #16328, #17297, #9264, .T. ) ;
#4583 = DIRECTION ( 'NONE',  ( 0.000000000000000000, -1.000000000000000000, 0.000000000000000000 ) ) ;
#4584 = AXIS2_PLACEMENT_3D ( 'NONE', #8855, #11835, #4704 ) ;
#4585 = AXIS2_PLACEMENT_3D ( 'NONE', #12321, #2016, #5199 ) ;
#4586 = DIRECTION ( 'NONE',  ( 0.000000000000000000, 0.000000000000000000, -1.000000000000000000 ) ) ;
#4587 = VERTEX_POINT ( 'NONE', #3191 ) ;
#4588 = ADVANCED_FACE ( 'NONE', ( #9088 ), #13116, .T. ) ;
#4589 = DIRECTION ( 'NONE',  ( 1.000000000000000000, 0.000000000000000000, 0.000000000000000000 ) ) ;
#4590 = CARTESIAN_POINT ( 'NONE',  ( -81.24478565583312673, -91.08423613455723000, 39.14322682088972272 ) ) ;
#4591 = LINE ( 'NONE', #1976, #17314 ) ;
#4592 = ORIENTED_EDGE ( 'NONE', *, *, #7062, .T. ) ;
#4593 = DIRECTION ( 'NONE',  ( -1.000000000000000000, 0.000000000000000000, 0.000000000000000000 ) ) ;
#4594 = DIRECTION ( 'NONE',  ( 0.000000000000000000, 0.000000000000000000, 1.000000000000000000 ) ) ;
#4595 = EDGE_CURVE ( 'NONE', #8085, #15750, #4591, .T. ) ;
#4596 = ORIENTED_EDGE ( 'NONE', *, *, #11100, .T. ) ;
#4597 = EDGE_CURVE ( 'NONE', #10621, #505, #4675, .T. ) ;
#4598 = PRODUCT_DEFINITION_FORMATION_WITH_SPECIFIED_SOURCE ( 'ANY', '', #6207, .NOT_KNOWN. ) ;
#4599 = AXIS2_PLACEMENT_3D ( 'NONE', #7553, #15974, #17640 ) ;
#4600 = CIRCLE ( 'NONE', #12396, 4.599999999999992539 ) ;
#4601 = EDGE_LOOP ( 'NONE', ( #2614, #8320, #15118, #1286, #11380, #11831, #2461, #5985 ) ) ;
#4602 = CARTESIAN_POINT ( 'NONE',  ( -57.08002265617300708, 84.22855780814606419, 15.00000000000006928 ) ) ;
#4603 = EDGE_CURVE ( 'NONE', #1908, #12880, #7466, .T. ) ;
#4604 = CARTESIAN_POINT ( 'NONE',  ( -57.08002265617300708, 84.22855780814606419, -15.00000000000001421 ) ) ;
#4605 = LINE ( 'NONE', #15667, #14693 ) ;
#4606 = VECTOR ( 'NONE', #8460, 1000.000000000000000 ) ;
#4607 = EDGE_LOOP ( 'NONE', ( #4521, #6484, #901, #5629 ) ) ;
#4608 = VECTOR ( 'NONE', #18115, 1000.000000000000000 ) ;
#4609 = CARTESIAN_POINT ( 'NONE',  ( -68.99615306438100504, 42.85071613813029501, -167.1454815528550739 ) ) ;
#4610 = CARTESIAN_POINT ( 'NONE',  ( -36.03642545851250389, 84.22855780814606419, -62.50000000000000000 ) ) ;
#4611 = FACE_OUTER_BOUND ( 'NONE', #11896, .T. ) ;
#4612 = CARTESIAN_POINT ( 'NONE',  ( -71.24615306438100504, 50.84170520456370923, 15.00000000000006928 ) ) ;
#4613 = VERTEX_POINT ( 'NONE', #7955 ) ;
#4614 = VECTOR ( 'NONE', #10031, 999.9999999999998863 ) ;
#4615 = PLANE ( 'NONE',  #13735 ) ;
#4616 = VERTEX_POINT ( 'NONE', #4035 ) ;
#4617 = CARTESIAN_POINT ( 'NONE',  ( -63.91856434051376823, 76.59466308582156557, -167.1454815528550739 ) ) ;
#4618 = ORIENTED_EDGE ( 'NONE', *, *, #8832, .F. ) ;
#4619 = CIRCLE ( 'NONE', #18384, 4.599999999999992539 ) ;
#4620 = ORIENTED_EDGE ( 'NONE', *, *, #156, .T. ) ;
#4621 = AXIS2_PLACEMENT_3D ( 'NONE', #13252, #8949, #4540 ) ;
#4622 = AXIS2_PLACEMENT_3D ( 'NONE', #13944, #6534, #1037 ) ;
#4623 = DIRECTION ( 'NONE',  ( 0.000000000000000000, 1.000000000000000000, 0.000000000000000000 ) ) ;
#4624 = LINE ( 'NONE', #11741, #5484 ) ;
#4625 = ORIENTED_EDGE ( 'NONE', *, *, #18094, .T. ) ;
#4626 = DIRECTION ( 'NONE',  ( 1.000000000000000000, 0.000000000000000000, 0.000000000000000000 ) ) ;
#4627 = DIRECTION ( 'NONE',  ( -5.204170427930409450E-16, 0.000000000000000000, 1.000000000000000000 ) ) ;
#4628 = DIRECTION ( 'NONE',  ( -1.000000000000000000, 0.000000000000000000, 0.000000000000000000 ) ) ;
#4629 = VERTEX_POINT ( 'NONE', #18247 ) ;
#4630 = ADVANCED_FACE ( 'NONE', ( #3748 ), #15056, .F. ) ;
#4631 = DIRECTION ( 'NONE',  ( 0.000000000000000000, 1.000000000000000000, 0.000000000000000000 ) ) ;
#4632 = CARTESIAN_POINT ( 'NONE',  ( -67.46561775476841660, 81.24207102880470188, 15.00000000000006928 ) ) ;
#4633 = CARTESIAN_POINT ( 'NONE',  ( -71.24615306438100504, 50.84170520456370923, -167.1454815528550739 ) ) ;
#4634 = ORIENTED_EDGE ( 'NONE', *, *, #3689, .F. ) ;
#4635 = AXIS2_PLACEMENT_3D ( 'NONE', #7678, #1784, #389 ) ;
#4636 = EDGE_CURVE ( 'NONE', #4073, #2148, #6640, .T. ) ;
#4637 = AXIS2_PLACEMENT_3D ( 'NONE', #17833, #3898, #3720 ) ;
#4638 = AXIS2_PLACEMENT_3D ( 'NONE', #7114, #12821, #11420 ) ;
#4639 = FACE_OUTER_BOUND ( 'NONE', #12369, .T. ) ;
#4640 = LINE ( 'NONE', #13625, #9892 ) ;
#4641 = ORIENTED_EDGE ( 'NONE', *, *, #16668, .F. ) ;
#4642 = ORIENTED_EDGE ( 'NONE', *, *, #6772, .F. ) ;
#4643 = B_SPLINE_CURVE_WITH_KNOTS ( 'NONE', 3,
 ( #18150, #5319, #1127, #6825, #5876, #10101, #2987, #8610, #266, #18442 ),
 .UNSPECIFIED., .F., .F.,
 ( 4, 2, 2, 2, 4 ),
 ( 0.0003974689443029659507, 0.008237140244579449141, 0.01019705806964857006, 0.01215697589471769098, 0.01607681154485594496 ),
 .UNSPECIFIED. ) ;
#4644 = VERTEX_POINT ( 'NONE', #3832 ) ;
#4645 = DIRECTION ( 'NONE',  ( -5.204170427930409450E-16, 0.000000000000000000, 1.000000000000000000 ) ) ;
#4646 = CARTESIAN_POINT ( 'NONE',  ( -114.6648972341095885, 110.5691553257988602, 26.35917033480640725 ) ) ;
#4647 = CARTESIAN_POINT ( 'NONE',  ( -66.13756785686383921, 112.1658165091852908, -26.33995503696884910 ) ) ;
#4648 =( REPRESENTATION_RELATIONSHIP ('NONE','NONE', #359, #16862 ) REPRESENTATION_RELATIONSHIP_WITH_TRANSFORMATION ( #3866 )SHAPE_REPRESENTATION_RELATIONSHIP( ) );
#4649 = DIRECTION ( 'NONE',  ( 1.000000000000000000, 0.000000000000000000, 0.000000000000000000 ) ) ;
#4650 = CARTESIAN_POINT ( 'NONE',  ( -68.99615306438067819, 145.9084177316626949, -15.00000000000001421 ) ) ;
#4651 = ORIENTED_EDGE ( 'NONE', *, *, #2655, .F. ) ;
#4652 = CARTESIAN_POINT ( 'NONE',  ( -61.98611128973170992, 74.59995546124152099, -167.1454815528550739 ) ) ;
#4653 = DIRECTION ( 'NONE',  ( 0.000000000000000000, 0.000000000000000000, -1.000000000000000000 ) ) ;
#4654 = CARTESIAN_POINT ( 'NONE',  ( -57.08002265617302839, 27.37185818390810965, 97.49999999999998579 ) ) ;
#4655 = DIRECTION ( 'NONE',  ( 0.000000000000000000, 0.000000000000000000, -1.000000000000000000 ) ) ;
#4656 = CARTESIAN_POINT ( 'NONE',  ( -36.03642545851251100, 84.22855780814606419, 70.00000000000001421 ) ) ;
#4657 = DIRECTION ( 'NONE',  ( 0.000000000000000000, 1.000000000000000000, 0.000000000000000000 ) ) ;
#4658 = ORIENTED_EDGE ( 'NONE', *, *, #10520, .T. ) ;
#4659 = EDGE_CURVE ( 'NONE', #13953, #12828, #17629, .T. ) ;
#4660 = CARTESIAN_POINT ( 'NONE',  ( -60.62932119839002354, 94.43552448259767118, 15.00000000000006928 ) ) ;
#4661 = CARTESIAN_POINT ( 'NONE',  ( -36.03642545851251100, 84.22855780814606419, 55.00000000000001421 ) ) ;
#4662 = VERTEX_POINT ( 'NONE', #9539 ) ;
#4663 = ORIENTED_EDGE ( 'NONE', *, *, #8830, .T. ) ;
#4664 = ORIENTED_EDGE ( 'NONE', *, *, #250, .F. ) ;
#4665 = CARTESIAN_POINT ( 'NONE',  ( -68.99615306438106188, 26.52789703166272162, 15.00000000000006928 ) ) ;
#4666 = CARTESIAN_POINT ( 'NONE',  ( -68.99615306438089135, 83.07656473166271383, -15.00000000000001421 ) ) ;
#4667 = EDGE_CURVE ( 'NONE', #2433, #16663, #2432, .T. ) ;
#4668 = CARTESIAN_POINT ( 'NONE',  ( -123.4618227840623632, -151.5628872026273086, -18.23991632971910803 ) ) ;
#4669 = CARTESIAN_POINT ( 'NONE',  ( -71.24615306438079188, 104.2487802545637408, -15.00000000000001421 ) ) ;
#4670 = CYLINDRICAL_SURFACE ( 'NONE', #17317, 20.99999999999999645 ) ;
#4671 = CARTESIAN_POINT ( 'NONE',  ( -44.59353464447068660, 84.80960611389554060, 15.00000000000006928 ) ) ;
#4672 = ORIENTED_EDGE ( 'NONE', *, *, #16691, .F. ) ;
#4673 = PLANE ( 'NONE',  #5105 ) ;
#4674 = CARTESIAN_POINT ( 'NONE',  ( -68.99615306438100504, 39.09426763166271002, 15.00000000000006928 ) ) ;
#4675 = LINE ( 'NONE', #6076, #15539 ) ;
#4676 = ORIENTED_EDGE ( 'NONE', *, *, #10256, .F. ) ;
#4677 = ADVANCED_FACE ( 'NONE', ( #17952 ), #10955, .F. ) ;
#4678 = EDGE_CURVE ( 'NONE', #2791, #11538, #2147, .T. ) ;
#4679 = DIRECTION ( 'NONE',  ( 0.000000000000000000, 1.000000000000000000, -0.000000000000000000 ) ) ;
#4680 = LINE ( 'NONE', #2630, #14598 ) ;
#4681 = ORIENTED_EDGE ( 'NONE', *, *, #15039, .F. ) ;
#4682 = EDGE_CURVE ( 'NONE', #677, #17987, #9639, .T. ) ;
#4683 = PLANE ( 'NONE',  #11803 ) ;
#4684 = EDGE_CURVE ( 'NONE', #513, #12828, #5077, .T. ) ;
#4685 = LINE ( 'NONE', #14792, #12987 ) ;
#4686 = CARTESIAN_POINT ( 'NONE',  ( -70.71978124295668522, -91.08423613455721579, -28.18308811886538479 ) ) ;
#4687 = ORIENTED_EDGE ( 'NONE', *, *, #11548, .T. ) ;
#4688 = EDGE_CURVE ( 'NONE', #16652, #15808, #5323, .T. ) ;
#4689 = EDGE_CURVE ( 'NONE', #18116, #3150, #3927, .T. ) ;
#4690 = ORIENTED_EDGE ( 'NONE', *, *, #14068, .F. ) ;
#4691 = CYLINDRICAL_SURFACE ( 'NONE', #332, 10.24900000000001477 ) ;
#4692 = DIRECTION ( 'NONE',  ( 0.000000000000000000, 0.000000000000000000, 1.000000000000000000 ) ) ;
#4693 = CARTESIAN_POINT ( 'NONE',  ( -123.4618227840623632, -111.0842361345572158, 57.00000000000000000 ) ) ;
#4694 = DIRECTION ( 'NONE',  ( 1.156482317317869999E-16, 0.000000000000000000, 1.000000000000000000 ) ) ;
#4695 = ORIENTED_EDGE ( 'NONE', *, *, #12077, .F. ) ;
#4696 = CARTESIAN_POINT ( 'NONE',  ( -123.4618227840623632, 84.22855780814606419, 70.00000000000001421 ) ) ;
#4697 = VERTEX_POINT ( 'NONE', #13666 ) ;
#4698 = EDGE_CURVE ( 'NONE', #4736, #9544, #5378, .T. ) ;
#4699 = CARTESIAN_POINT ( 'NONE',  ( -123.4618227840623632, 84.22855780814606419, 62.50000000000001421 ) ) ;
#4700 = VERTEX_POINT ( 'NONE', #12365 ) ;
#4701 = ORIENTED_EDGE ( 'NONE', *, *, #15545, .T. ) ;
#4702 = DIRECTION ( 'NONE',  ( -1.000000000000000000, -0.000000000000000000, -0.000000000000000000 ) ) ;
#4703 = DIRECTION ( 'NONE',  ( 0.9240607556974789194, -0.3822456275483139820, 0.000000000000000000 ) ) ;
#4704 = DIRECTION ( 'NONE',  ( 0.000000000000000000, 0.000000000000000000, -1.000000000000000000 ) ) ;
#4705 = EDGE_LOOP ( 'NONE', ( #17288, #12237, #5225, #13510 ) ) ;
#4706 = CARTESIAN_POINT ( 'NONE',  ( -59.05157857372951469, 96.57209730311865314, -15.00000000000001421 ) ) ;
#4707 = CYLINDRICAL_SURFACE ( 'NONE', #2743, 4.599999999999999645 ) ;
#4708 = ADVANCED_FACE ( 'NONE', ( #11043 ), #16451, .T. ) ;
#4709 = FACE_OUTER_BOUND ( 'NONE', #9933, .T. ) ;
#4710 = ORIENTED_EDGE ( 'NONE', *, *, #7236, .T. ) ;
#4711 = FACE_OUTER_BOUND ( 'NONE', #13237, .T. ) ;
#4712 = CARTESIAN_POINT ( 'NONE',  ( -68.99615306438089135, 86.21815738166266385, 15.00000000000006928 ) ) ;
#4713 = CARTESIAN_POINT ( 'NONE',  ( -100.4870060002411805, -151.5628872026273086, -57.00000000000000000 ) ) ;
#4714 = ORIENTED_EDGE ( 'NONE', *, *, #8572, .F. ) ;
#4715 = CYLINDRICAL_SURFACE ( 'NONE', #4621, 10.24900000000000055 ) ;
#4716 = VECTOR ( 'NONE', #8353, 1000.000000000000000 ) ;
#4717 = CYLINDRICAL_SURFACE ( 'NONE', #15210, 4.600000000000006750 ) ;
#4718 = VERTEX_POINT ( 'NONE', #12170 ) ;
#4719 = ORIENTED_EDGE ( 'NONE', *, *, #7223, .T. ) ;
#4720 = EDGE_LOOP ( 'NONE', ( #2627, #14260 ) ) ;
#4721 = CARTESIAN_POINT ( 'NONE',  ( -67.46561775476841660, 81.24207102880470188, -167.1454815528550739 ) ) ;
#4722 = DIRECTION ( 'NONE',  ( 1.000000000000000000, 0.000000000000000000, 0.000000000000000000 ) ) ;
#4723 = CARTESIAN_POINT ( 'NONE',  ( -71.24615306438111872, 21.67850061522927518, -15.00000000000001421 ) ) ;
#4724 = SHAPE_REPRESENTATION_RELATIONSHIP ( 'NONE' , 'NONE' ,  #13055, #7691 ) ;
#4725 = DIRECTION ( 'NONE',  ( 0.000000000000000000, 0.000000000000000000, 1.000000000000000000 ) ) ;
#4726 = CIRCLE ( 'NONE', #1459, 20.99999999999998934 ) ;
#4727 = DIRECTION ( 'NONE',  ( 1.000000000000000000, 0.000000000000000000, 0.000000000000000000 ) ) ;
#4728 = ORIENTED_EDGE ( 'NONE', *, *, #17495, .F. ) ;
#4729 = DIRECTION ( 'NONE',  ( 1.000000000000000000, 0.000000000000000000, 0.000000000000000000 ) ) ;
#4730 = DIRECTION ( 'NONE',  ( 1.000000000000000000, 0.000000000000000000, 0.000000000000000000 ) ) ;
#4731 = CARTESIAN_POINT ( 'NONE',  ( -68.99615306438084872, 74.26664263813026423, 15.00000000000006928 ) ) ;
#4732 = FACE_OUTER_BOUND ( 'NONE', #18389, .T. ) ;
#4733 = CARTESIAN_POINT ( 'NONE',  ( -37.17548309439882104, 91.05880801963004956, 65.60778368822992945 ) ) ;
#4734 = EDGE_LOOP ( 'NONE', ( #16114, #13054, #1104, #1885 ) ) ;
#4735 = FACE_OUTER_BOUND ( 'NONE', #8532, .T. ) ;
#4736 = VERTEX_POINT ( 'NONE', #13853 ) ;
#4737 = DIRECTION ( 'NONE',  ( -5.204170427930409450E-16, 0.000000000000000000, 1.000000000000000000 ) ) ;
#4738 = DIRECTION ( 'NONE',  ( 1.156482317317869999E-16, 0.000000000000000000, 1.000000000000000000 ) ) ;
#4739 = EDGE_LOOP ( 'NONE', ( #17459, #9782, #11299, #2720 ) ) ;
#4740 = VECTOR ( 'NONE', #17220, 1000.000000000000000 ) ;
#4741 = ADVANCED_FACE ( 'NONE', ( #5238, #6539 ), #16548, .T. ) ;
#4742 = VERTEX_POINT ( 'NONE', #17859 ) ;
#4743 = VECTOR ( 'NONE', #252, 1000.000000000000000 ) ;
#4744 = ORIENTED_EDGE ( 'NONE', *, *, #18315, .T. ) ;
#4745 = DIRECTION ( 'NONE',  ( -0.000000000000000000, -0.000000000000000000, -1.000000000000000000 ) ) ;
#4746 = CARTESIAN_POINT ( 'NONE',  ( -71.24615306438097662, 62.51920506522922949, -15.00000000000001421 ) ) ;
#4747 = CARTESIAN_POINT ( 'NONE',  ( -77.53293207630810002, 79.27386099610181702, 68.13566487288508711 ) ) ;
#4748 = CARTESIAN_POINT ( 'NONE',  ( -57.08002265617300708, 84.22855780814606419, -47.50000000000000000 ) ) ;
#4749 = FACE_OUTER_BOUND ( 'NONE', #17039, .T. ) ;
#4750 = DIRECTION ( 'NONE',  ( 0.000000000000000000, 1.000000000000000000, 0.000000000000000000 ) ) ;
#4751 = CARTESIAN_POINT ( 'NONE',  ( -67.59262256747315689, 0.000000000000000000, 0.000000000000000000 ) ) ;
#4752 = ORIENTED_EDGE ( 'NONE', *, *, #13167, .F. ) ;
#4753 = AXIS2_PLACEMENT_3D ( 'NONE', #6787, #11091, #15188 ) ;
#4754 = CARTESIAN_POINT ( 'NONE',  ( -46.00691148729628566, 49.61991837646342418, -27.56955468854675928 ) ) ;
#4755 = PLANE ( 'NONE',  #13247 ) ;
#4756 = CIRCLE ( 'NONE', #1789, 3.999999999999996447 ) ;
#4757 = CARTESIAN_POINT ( 'NONE',  ( -71.24615306438090556, 79.11603905456372843, -15.00000000000001421 ) ) ;
#4758 = ORIENTED_EDGE ( 'NONE', *, *, #10967, .T. ) ;
#4759 = DIRECTION ( 'NONE',  ( 0.000000000000000000, 0.000000000000000000, 1.000000000000000000 ) ) ;
#4760 = DIRECTION ( 'NONE',  ( 1.000000000000000000, 0.000000000000000000, 0.000000000000000000 ) ) ;
#4761 = ORIENTED_EDGE ( 'NONE', *, *, #8356, .F. ) ;
#4762 = VECTOR ( 'NONE', #11448, 1000.000000000000000 ) ;
#4763 = ORIENTED_EDGE ( 'NONE', *, *, #376, .T. ) ;
#4764 = VECTOR ( 'NONE', #9735, 1000.000000000000000 ) ;
#4765 = AXIS2_PLACEMENT_3D ( 'NONE', #15733, #5700, #5794 ) ;
#4766 = DIRECTION ( 'NONE',  ( -5.204170427930409450E-16, 0.000000000000000000, 1.000000000000000000 ) ) ;
#4767 = DIRECTION ( 'NONE',  ( 0.000000000000000000, 0.000000000000000000, -1.000000000000000000 ) ) ;
#4768 = CARTESIAN_POINT ( 'NONE',  ( -68.99615306438100504, 48.51904558166270220, 15.00000000000006928 ) ) ;
#4769 = ORIENTED_EDGE ( 'NONE', *, *, #822, .T. ) ;
#4770 = EDGE_CURVE ( 'NONE', #881, #8164, #13756, .T. ) ;
#4771 = DIRECTION ( 'NONE',  ( -1.000000000000000000, -2.062304371594500740E-16, 0.000000000000000000 ) ) ;
#4772 = ORIENTED_EDGE ( 'NONE', *, *, #3097, .T. ) ;
#4773 = EDGE_CURVE ( 'NONE', #16002, #4147, #14648, .T. ) ;
#4774 = CARTESIAN_POINT ( 'NONE',  ( -70.71978124295696944, -91.08423613455721579, 5.204170427930421283E-15 ) ) ;
#4775 = DIRECTION ( 'NONE',  ( 1.047634945911799279E-14, 0.000000000000000000, -1.000000000000000000 ) ) ;
#4776 = CARTESIAN_POINT ( 'NONE',  ( -77.26346150264693335, 90.19024662095813483, 57.92355293790617310 ) ) ;
#4777 = AXIS2_PLACEMENT_3D ( 'NONE', #4293, #15715, #8411 ) ;
#4778 = CARTESIAN_POINT ( 'NONE',  ( -67.59262256747315689, 50.58224449241410525, -15.00000000000000711 ) ) ;
#4779 = EDGE_LOOP ( 'NONE', ( #4786, #3174, #15655, #17331 ) ) ;
#4780 = VECTOR ( 'NONE', #12460, 1000.000000000000000 ) ;
#4781 = LINE ( 'NONE', #17698, #10736 ) ;
#4782 = VERTEX_POINT ( 'NONE', #4214 ) ;
#4784 = EDGE_CURVE ( 'NONE', #17387, #13044, #8616, .T. ) ;
#4783 = AXIS2_PLACEMENT_3D ( 'NONE', #6711, #7093, #15307 ) ;
#4785 = LINE ( 'NONE', #6100, #5908 ) ;
#4786 = ORIENTED_EDGE ( 'NONE', *, *, #14642, .F. ) ;
#4787 = AXIS2_PLACEMENT_3D ( 'NONE', #9615, #15509, #5590 ) ;
#4788 = EDGE_CURVE ( 'NONE', #2374, #11152, #2913, .T. ) ;
#4789 = ADVANCED_FACE ( 'NONE', ( #2626 ), #14318, .T. ) ;
#4790 = EDGE_LOOP ( 'NONE', ( #18408, #8428, #10519, #15677 ) ) ;
#4791 = ORIENTED_EDGE ( 'NONE', *, *, #18301, .F. ) ;
#4792 = VECTOR ( 'NONE', #1631, 1000.000000000000000 ) ;
#4793 = CARTESIAN_POINT ( 'NONE',  ( -92.59262256747321373, 117.8748711238780373, 35.00000000000000000 ) ) ;
#4794 = CARTESIAN_POINT ( 'NONE',  ( -36.03642545851251100, 84.22855780814606419, 70.00000000000001421 ) ) ;
#4795 = EDGE_CURVE ( 'NONE', #2797, #11084, #8389, .T. ) ;
#4796 = EDGE_LOOP ( 'NONE', ( #12549, #5812 ) ) ;
#4797 = EDGE_CURVE ( 'NONE', #18335, #8753, #17291, .T. ) ;
#4798 = ADVANCED_FACE ( 'NONE', ( #16935 ), #8533, .T. ) ;
#4799 = VECTOR ( 'NONE', #11184, 1000.000000000000000 ) ;
#4800 = LINE ( 'NONE', #7981, #17071 ) ;
#4801 = DIRECTION ( 'NONE',  ( 0.000000000000000000, 0.000000000000000000, 1.000000000000000000 ) ) ;
#4802 = ORIENTED_EDGE ( 'NONE', *, *, #3002, .T. ) ;
#4803 = EDGE_CURVE ( 'NONE', #11561, #2867, #3906, .T. ) ;
#4804 = DIRECTION ( 'NONE',  ( 0.000000000000000000, 1.000000000000000000, 0.000000000000000000 ) ) ;
#4805 = ORIENTED_EDGE ( 'NONE', *, *, #11565, .T. ) ;
#4806 = DIRECTION ( 'NONE',  ( 1.000000000000000000, 0.000000000000000000, 0.000000000000000000 ) ) ;
#4807 = ORIENTED_EDGE ( 'NONE', *, *, #10752, .F. ) ;
#4808 = AXIS2_PLACEMENT_3D ( 'NONE', #9285, #9466, #3946 ) ;
#4809 = CARTESIAN_POINT ( 'NONE',  ( -107.5926225674731853, 50.58224449241411236, 35.00000000000000000 ) ) ;
#4810 = CARTESIAN_POINT ( 'NONE',  ( -76.37409655828220423, -95.65021661331557823, -45.05044770573186952 ) ) ;
#4811 = AXIS2_PLACEMENT_3D ( 'NONE', #17794, #1898, #14888 ) ;
#4812 = VECTOR ( 'NONE', #16001, 1000.000000000000000 ) ;
#4813 = EDGE_LOOP ( 'NONE', ( #13052, #9623, #3419, #5022 ) ) ;
#4814 = EDGE_CURVE ( 'NONE', #8556, #18489, #1416, .T. ) ;
#4815 = ADVANCED_FACE ( 'NONE', ( #15443 ), #11424, .T. ) ;
#4816 = ORIENTED_EDGE ( 'NONE', *, *, #11450, .T. ) ;
#4817 = ORIENTED_EDGE ( 'NONE', *, *, #10762, .T. ) ;
#4818 = CARTESIAN_POINT ( 'NONE',  ( -71.24615306438094819, 66.54966845456371516, -167.1454815528550739 ) ) ;
#4819 = DIRECTION ( 'NONE',  ( -1.000000000000000000, -0.000000000000000000, -0.000000000000000000 ) ) ;
#4820 = AXIS2_PLACEMENT_3D ( 'NONE', #169, #11653, #17264 ) ;
#4821 = ORIENTED_EDGE ( 'NONE', *, *, #10984, .F. ) ;
#4822 = APPLICATION_PROTOCOL_DEFINITION ( 'draft international standard', 'automotive_design', 1998, #3453 ) ;
#4823 = CARTESIAN_POINT ( 'NONE',  ( -57.08002265617300708, 84.22855780814606419, -167.1454815528550739 ) ) ;
#4824 = CARTESIAN_POINT ( 'NONE',  ( -57.08002265617300708, 84.22855780814606419, 92.50000000000000000 ) ) ;
#4825 = LINE ( 'NONE', #11855, #12696 ) ;
#4826 = ORIENTED_EDGE ( 'NONE', *, *, #10987, .F. ) ;
#4827 = CARTESIAN_POINT ( 'NONE',  ( -50.81952187608693805, 73.40930968350535579, -15.00000000000001421 ) ) ;
#4828 = AXIS2_PLACEMENT_3D ( 'NONE', #428, #6116, #6200 ) ;
#4829 = AXIS2_PLACEMENT_3D ( 'NONE', #2624, #9534, #16723 ) ;
#4830 = LINE ( 'NONE', #9233, #8246 ) ;
#4831 = DIRECTION ( 'NONE',  ( 1.000000000000000000, 0.000000000000000000, 0.000000000000000000 ) ) ;
#4832 = DIRECTION ( 'NONE',  ( -1.000000000000000000, 0.000000000000000000, 0.000000000000000000 ) ) ;
#4833 = CARTESIAN_POINT ( 'NONE',  ( -45.39578445746348478, 88.67024416760654049, -167.1454815528550739 ) ) ;
#4834 = ORIENTED_EDGE ( 'NONE', *, *, #3642, .F. ) ;
#4835 = CARTESIAN_POINT ( 'NONE',  ( -53.97067643794850511, 72.12145385653101926, -167.1454815528550739 ) ) ;
#4836 = CARTESIAN_POINT ( 'NONE',  ( -68.99615306438074924, 120.7756765316626542, -15.00000000000001421 ) ) ;
#4837 = ORIENTED_EDGE ( 'NONE', *, *, #13828, .F. ) ;
#4838 = EDGE_CURVE ( 'NONE', #4021, #8598, #15807, .T. ) ;
#4839 = VECTOR ( 'NONE', #13676, 1000.000000000000114 ) ;
#4840 = DIRECTION ( 'NONE',  ( 0.000000000000000000, 0.000000000000000000, 1.000000000000000000 ) ) ;
#4841 = CARTESIAN_POINT ( 'NONE',  ( -71.24615306438074924, 116.8151508545637398, 15.00000000000006928 ) ) ;
#4842 = ORIENTED_EDGE ( 'NONE', *, *, #6982, .T. ) ;
#4843 = ORIENTED_EDGE ( 'NONE', *, *, #9867, .T. ) ;
#4844 = VECTOR ( 'NONE', #9370, 1000.000000000000000 ) ;
#4845 = CIRCLE ( 'NONE', #3066, 20.99999999999999645 ) ;
#4846 = ORIENTED_EDGE ( 'NONE', *, *, #13981, .F. ) ;
#4847 = CARTESIAN_POINT ( 'NONE',  ( -107.5926225674731853, 110.5691553257988460, 30.35917033480641081 ) ) ;
#4848 = DIRECTION ( 'NONE',  ( -1.000000000000000000, 0.000000000000000000, 0.000000000000000000 ) ) ;
#4849 = CARTESIAN_POINT ( 'NONE',  ( -71.24615306438070661, 134.7758360152292312, -167.1454815528550739 ) ) ;
#4850 = CIRCLE ( 'NONE', #15644, 81.86696747278378439 ) ;
#4851 = LINE ( 'NONE', #15234, #11381 ) ;
#4852 = CARTESIAN_POINT ( 'NONE',  ( 5.699999999999996625, 2.220446049250299276E-16, 4.000000000000000000 ) ) ;
#4853 = CARTESIAN_POINT ( 'NONE',  ( -62.81538793034061285, 92.72253132893551708, 15.00000000000006928 ) ) ;
#4854 = ORIENTED_EDGE ( 'NONE', *, *, #1717, .T. ) ;
#4855 = EDGE_CURVE ( 'NONE', #1895, #12660, #8701, .T. ) ;
#4856 = CARTESIAN_POINT ( 'NONE',  ( -68.99615306438072082, 130.8153103381302742, -15.00000000000001421 ) ) ;
#4857 = CARTESIAN_POINT ( 'NONE',  ( -76.13473419340549242, 61.88023627570096608, -26.63205224474248922 ) ) ;
#4858 = AXIS2_PLACEMENT_3D ( 'NONE', #10842, #13561, #751 ) ;
#4859 = VECTOR ( 'NONE', #16547, 1000.000000000000000 ) ;
#4860 = AXIS2_PLACEMENT_3D ( 'NONE', #832, #3454, #5028 ) ;
#4861 = DIRECTION ( 'NONE',  ( 0.000000000000000000, 0.000000000000000000, -1.000000000000000000 ) ) ;
#4862 = ORIENTED_EDGE ( 'NONE', *, *, #16573, .F. ) ;
#4863 = EDGE_CURVE ( 'NONE', #4629, #12641, #10023, .T. ) ;
#4864 = CYLINDRICAL_SURFACE ( 'NONE', #544, 4.600000000000006750 ) ;
#4865 = ORIENTED_EDGE ( 'NONE', *, *, #1831, .T. ) ;
#4866 = AXIS2_PLACEMENT_3D ( 'NONE', #2068, #9276, #16369 ) ;
#4867 = AXIS2_PLACEMENT_3D ( 'NONE', #12891, #14204, #5579 ) ;
#4868 = VERTEX_POINT ( 'NONE', #11330 ) ;
#4869 = CIRCLE ( 'NONE', #7281, 0.4000000000000001887 ) ;
#4870 = VECTOR ( 'NONE', #15384, 1000.000000000000000 ) ;
#4871 = DIRECTION ( 'NONE',  ( 0.000000000000000000, 0.000000000000000000, 1.000000000000000000 ) ) ;
#4872 = LINE ( 'NONE', #5151, #1572 ) ;
#4873 = CARTESIAN_POINT ( 'NONE',  ( -49.40461175531926585, 94.09456345901895702, 15.00000000000006928 ) ) ;
#4874 = FACE_OUTER_BOUND ( 'NONE', #7173, .T. ) ;
#4875 = ORIENTED_EDGE ( 'NONE', *, *, #8488, .F. ) ;
#4876 = DIRECTION ( 'NONE',  ( -1.000000000000000000, 0.000000000000000000, 1.156482317317869999E-16 ) ) ;
#4877 = DIRECTION ( 'NONE',  ( -0.9915318908039647550, 0.000000000000000000, 0.1298634264091108326 ) ) ;
#4878 = VERTEX_POINT ( 'NONE', #4396 ) ;
#4879 = DIRECTION ( 'NONE',  ( 0.000000000000000000, 0.000000000000000000, 1.000000000000000000 ) ) ;
#4880 = DIRECTION ( 'NONE',  ( -1.000000000000000000, -0.000000000000000000, -0.000000000000000000 ) ) ;
#4881 = DIRECTION ( 'NONE',  ( -1.000000000000000000, 0.000000000000000000, 0.000000000000000000 ) ) ;
#4882 = DIRECTION ( 'NONE',  ( 0.000000000000000000, 1.000000000000000000, 0.000000000000000000 ) ) ;
#4883 = ORIENTED_EDGE ( 'NONE', *, *, #4682, .F. ) ;
#4884 = LINE ( 'NONE', #8922, #16698 ) ;
#4885 = ORIENTED_EDGE ( 'NONE', *, *, #3317, .F. ) ;
#4886 = AXIS2_PLACEMENT_3D ( 'NONE', #9230, #16613, #17917 ) ;
#4887 = CARTESIAN_POINT ( 'NONE',  ( -68.99615306438089135, 80.54982793813027797, -167.1454815528550739 ) ) ;
#4889 = ORIENTED_EDGE ( 'NONE', *, *, #17853, .F. ) ;
#4888 = VECTOR ( 'NONE', #771, 1000.000000000000000 ) ;
#4890 = PRODUCT_DEFINITION_SHAPE ( 'NONE', 'NONE',  #2227 ) ;
#4891 = EDGE_CURVE ( 'NONE', #11152, #11410, #7298, .T. ) ;
#4892 = ORIENTED_EDGE ( 'NONE', *, *, #2972, .T. ) ;
#4893 = CARTESIAN_POINT ( 'NONE',  ( -71.24615306438076345, 131.6342433652292243, -167.1454815528550739 ) ) ;
#4894 = CARTESIAN_POINT ( 'NONE',  ( -208.2552686774341737, 84.22855780814606419, 62.50000000000001421 ) ) ;
#4895 = VECTOR ( 'NONE', #11384, 1000.000000000000000 ) ;
#4896 = VERTEX_POINT ( 'NONE', #14405 ) ;
#4897 = CIRCLE ( 'NONE', #1667, 12.50000000000000355 ) ;
#4898 = VECTOR ( 'NONE', #4442, 1000.000000000000000 ) ;
#4899 = AXIS2_PLACEMENT_3D ( 'NONE', #7476, #13196, #17482 ) ;
#4900 = LINE ( 'NONE', #13696, #1251 ) ;
#4901 = ADVANCED_FACE ( 'NONE', ( #1585 ), #192, .F. ) ;
#4902 = CARTESIAN_POINT ( 'NONE',  ( -68.99615306438089135, 67.98345733813025049, 15.00000000000006928 ) ) ;
#4903 = ORIENTED_EDGE ( 'NONE', *, *, #18024, .F. ) ;
#4904 = EDGE_CURVE ( 'NONE', #8741, #13368, #12755, .T. ) ;
#4905 = DIRECTION ( 'NONE',  ( 0.000000000000000000, 1.000000000000000000, -0.000000000000000000 ) ) ;
#4906 = ORIENTED_EDGE ( 'NONE', *, *, #6411, .T. ) ;
#4907 = CARTESIAN_POINT ( 'NONE',  ( -107.5926225674731711, 54.12595869546677818, -25.00000000000000000 ) ) ;
#4908 = PLANE ( 'NONE',  #15609 ) ;
#4909 = COLOUR_RGB ( '',0.7921568627450980005, 0.8196078431372548767, 0.9333333333333333481 ) ;
#4910 = LINE ( 'NONE', #4809, #7604 ) ;
#4911 = CIRCLE ( 'NONE', #15976, 12.50000000000001066 ) ;
#4912 = ADVANCED_FACE ( 'NONE', ( #6927 ), #18446, .F. ) ;
#4913 = EDGE_CURVE ( 'NONE', #5159, #9970, #15984, .T. ) ;
#4914 = CARTESIAN_POINT ( 'NONE',  ( -79.54423376290921510, -91.42293805878655633, -41.30286037549884526 ) ) ;
#4915 = VECTOR ( 'NONE', #9737, 1000.000000000000000 ) ;
#4916 = ORIENTED_EDGE ( 'NONE', *, *, #466, .F. ) ;
#4917 = AXIS2_PLACEMENT_3D ( 'NONE', #1218, #3743, #13846 ) ;
#4918 = ORIENTED_EDGE ( 'NONE', *, *, #8767, .T. ) ;
#4919 = ORIENTED_EDGE ( 'NONE', *, *, #10289, .T. ) ;
#4920 = DIRECTION ( 'NONE',  ( -0.9396926207859068736, 0.3420201433256725987, -4.890320548438441017E-16 ) ) ;
#4921 = CARTESIAN_POINT ( 'NONE',  ( -102.4618227840623774, -151.5628872026273086, 36.00000000000000711 ) ) ;
#4922 = EDGE_CURVE ( 'NONE', #16527, #12968, #14499, .T. ) ;
#4923 = ORIENTED_EDGE ( 'NONE', *, *, #3907, .T. ) ;
#4924 = DIRECTION ( 'NONE',  ( 0.000000000000000000, 0.000000000000000000, 1.000000000000000000 ) ) ;
#4925 = CARTESIAN_POINT ( 'NONE',  ( -71.24615306438070661, 134.7758360152292312, 15.00000000000006928 ) ) ;
#4926 = EDGE_CURVE ( 'NONE', #7603, #11788, #11688, .T. ) ;
#4927 = CARTESIAN_POINT ( 'NONE',  ( -68.99615306438100504, 45.37745293166267402, -167.1454815528550739 ) ) ;
#4928 = ORIENTED_EDGE ( 'NONE', *, *, #15172, .T. ) ;
#4929 = VECTOR ( 'NONE', #15149, 1000.000000000000000 ) ;
#4930 = FACE_OUTER_BOUND ( 'NONE', #15374, .T. ) ;
#4931 = AXIS2_PLACEMENT_3D ( 'NONE', #4654, #10368, #9152 ) ;
#4932 = CARTESIAN_POINT ( 'NONE',  ( -70.27900850916093134, -47.21335801510345220, 15.00000000000008171 ) ) ;
#4933 = EDGE_CURVE ( 'NONE', #14988, #11134, #17927, .T. ) ;
#4934 = CARTESIAN_POINT ( 'NONE',  ( -100.4870060002411805, -151.5628872026273086, -18.23991632971910803 ) ) ;
#4935 = AXIS2_PLACEMENT_3D ( 'NONE', #10718, #7549, #10542 ) ;
#4936 = EDGE_CURVE ( 'NONE', #3955, #2953, #6887, .T. ) ;
#4937 = LINE ( 'NONE', #1012, #12629 ) ;
#4938 = EDGE_LOOP ( 'NONE', ( #9520, #17217, #16566, #17818 ) ) ;
#4939 = DIRECTION ( 'NONE',  ( 0.000000000000000000, 0.000000000000000000, 1.000000000000000000 ) ) ;
#4940 = FACE_OUTER_BOUND ( 'NONE', #15136, .T. ) ;
#4941 = ORIENTED_EDGE ( 'NONE', *, *, #14634, .F. ) ;
#4942 = EDGE_CURVE ( 'NONE', #9953, #3055, #14066, .T. ) ;
#4943 = CARTESIAN_POINT ( 'NONE',  ( -27.71117476891160081, 84.22855780814606419, 25.00000000000000355 ) ) ;
#4944 = DIRECTION ( 'NONE',  ( -1.000000000000000000, 0.000000000000000000, 0.000000000000000000 ) ) ;
#4945 = EDGE_LOOP ( 'NONE', ( #12875, #2162, #18139, #1356, #306, #7134, #3160, #10501, #16789, #4641, #11834, #504, #8194, #429, #18310, #9046 ) ) ;
#4946 = ORIENTED_EDGE ( 'NONE', *, *, #17172, .F. ) ;
#4947 = AXIS2_PLACEMENT_3D ( 'NONE', #13294, #473, #6150 ) ;
#4948 = VECTOR ( 'NONE', #6712, 1000.000000000000000 ) ;
#4949 = CARTESIAN_POINT ( 'NONE',  ( -68.99615306438104767, 14.57638228813024206, 15.00000000000006928 ) ) ;
#4950 = ORIENTED_EDGE ( 'NONE', *, *, #1456, .T. ) ;
#4951 = LINE ( 'NONE', #470, #1355 ) ;
#4952 = CARTESIAN_POINT ( 'NONE',  ( -68.99615306438077766, 118.2489397381302751, -167.1454815528550739 ) ) ;
#4953 = CARTESIAN_POINT ( 'NONE',  ( -73.87934070579318302, 108.3200415776840515, 23.04436415747560574 ) ) ;
#4954 = DIRECTION ( 'NONE',  ( -1.000000000000000000, 0.000000000000000000, 0.000000000000000000 ) ) ;
#4955 = CARTESIAN_POINT ( 'NONE',  ( 0.000000000000000000, 5.629165124598635828, -3.250000000000016875 ) ) ;
#4956 = FACE_OUTER_BOUND ( 'NONE', #11769, .T. ) ;
#4957 = ORIENTED_EDGE ( 'NONE', *, *, #18208, .F. ) ;
#4958 = CARTESIAN_POINT ( 'NONE',  ( -75.54870230859340552, 61.39300225715819437, -24.42246604956295286 ) ) ;
#4959 = FACE_OUTER_BOUND ( 'NONE', #11051, .T. ) ;
#4960 = EDGE_LOOP ( 'NONE', ( #17846, #1482, #13571, #760, #2469, #4270, #1733, #6395, #13078, #7571, #4084, #15416, #8259, #4247, #4919, #5276, #2826, #3481, #7473, #7987, #9116, #4892, #10325, #711, #1181, #869, #2183, #4138, #3853, #16104, #3531, #10402, #14983, #910, #7253, #10682, #8181, #13888, #724, #14254, #4295, #4107, #1226, #4334, #11139, #1312, #13698, #17677, #12230, #11315, #11106, #6448, #17021, #6294, #419, #13187, #5143, #18447, #13133, #18276, #3237, #15382, #5902, #4309, #3562, #15201, #1901, #3020, #8815, #10337, #13832, #1452, #7149, #11661, #1321, #5449, #2254, #14456, #14334, #3733, #9384, #4596, #282, #16026, #14950, #14336, #8829, #18133, #10516, #2578, #2897, #14825, #14633, #10014, #1384, #17929, #3794, #16129, #3304, #14672, #11824, #3933, #5419, #11486, #1964, #4918, #17349, #12116, #6464, #185, #7231, #12085, #4763, #9509, #7256, #8761, #4658, #501, #15081, #15866, #10328, #12087, #15406, #17545, #2459, #8538, #5615, #16944, #6536, #15591, #9147, #15010, #12556, #15608, #14325, #300, #13208, #2724, #3753, #14143, #18053, #790, #14733, #446, #12422, #12340, #1582, #4002, #12628, #8805, #14145, #5635, #5656, #14178, #7471, #12922, #3218, #17380, #17981, #18499, #6141, #16955, #13936, #10563, #12911, #5059, #6759, #15171, #978, #9310, #8575, #8300, #16437, #3683, #15043, #413, #167, #6864, #15114, #2007, #5967, #15585, #4326, #11291, #12061, #2829, #7661, #10133, #10674, #17738, #7840, #15463, #9814, #6604, #6964, #14868, #15040 ) ) ;
#4961 = LINE ( 'NONE', #14870, #12834 ) ;
#4962 = ORIENTED_EDGE ( 'NONE', *, *, #12503, .F. ) ;
#4963 = ORIENTED_EDGE ( 'NONE', *, *, #17276, .F. ) ;
#4964 = DIRECTION ( 'NONE',  ( 1.156482317317869999E-16, 0.000000000000000000, 1.000000000000000000 ) ) ;
#4965 = DIRECTION ( 'NONE',  ( -5.204170427930409450E-16, 0.000000000000000000, 1.000000000000000000 ) ) ;
#4966 = CARTESIAN_POINT ( 'NONE',  ( -40.00733709395555593, 54.39356007051860331, -24.23452569059776351 ) ) ;
#4967 = CARTESIAN_POINT ( 'NONE',  ( -71.24615306438117557, 5.970537365229261262, -167.1454815528550739 ) ) ;
#4968 = ORIENTED_EDGE ( 'NONE', *, *, #17392, .F. ) ;
#4969 = DIRECTION ( 'NONE',  ( 0.000000000000000000, -1.000000000000000000, 0.000000000000000000 ) ) ;
#4970 = VERTEX_POINT ( 'NONE', #13098 ) ;
#4971 = DIRECTION ( 'NONE',  ( 0.000000000000000000, 0.000000000000000000, 1.000000000000000000 ) ) ;
#4972 = CARTESIAN_POINT ( 'NONE',  ( -107.5926225674731853, 110.5691553257988460, -26.35917033480641436 ) ) ;
#4973 = DIRECTION ( 'NONE',  ( 0.000000000000000000, 0.000000000000000000, -1.000000000000000000 ) ) ;
#4974 = CARTESIAN_POINT ( 'NONE',  ( -115.4692715616777434, -94.42547395655697073, 5.919112368231092880 ) ) ;
#4975 = ORIENTED_EDGE ( 'NONE', *, *, #9355, .F. ) ;
#4976 = DIRECTION ( 'NONE',  ( 0.000000000000000000, 0.000000000000000000, -1.000000000000000000 ) ) ;
#4977 = ORIENTED_EDGE ( 'NONE', *, *, #4926, .T. ) ;
#4978 = CARTESIAN_POINT ( 'NONE',  ( -107.5926225674732137, 117.8748711238780373, 35.00000000000000000 ) ) ;
#4979 = VERTEX_POINT ( 'NONE', #3341 ) ;
#4980 = PRODUCT_DEFINITION ( 'UNKNOWN', '', #7010, #18457 ) ;
#4981 = EDGE_CURVE ( 'NONE', #15230, #2837, #363, .T. ) ;
#4982 = ORIENTED_EDGE ( 'NONE', *, *, #13373, .T. ) ;
#4983 = DIRECTION ( 'NONE',  ( 0.000000000000000000, 0.000000000000000000, 1.000000000000000000 ) ) ;
#4984 = CARTESIAN_POINT ( 'NONE',  ( -68.99615306438099083, 27.14275288813028553, 15.00000000000006928 ) ) ;
#4985 = ORIENTED_EDGE ( 'NONE', *, *, #485, .T. ) ;
#4986 = LINE ( 'NONE', #10797, #5094 ) ;
#4987 = CARTESIAN_POINT ( 'NONE',  ( -212.2032458117903104, 84.22855780814606419, 62.50000000000001421 ) ) ;
#4988 = ORIENTED_EDGE ( 'NONE', *, *, #16020, .T. ) ;
#4989 = EDGE_CURVE ( 'NONE', #8149, #16609, #16256, .T. ) ;
#4990 = DIRECTION ( 'NONE',  ( 1.000000000000000000, 0.000000000000000000, 3.771137991253934490E-16 ) ) ;
#4991 = ORIENTED_EDGE ( 'NONE', *, *, #15221, .F. ) ;
#4992 = CARTESIAN_POINT ( 'NONE',  ( -71.24615306438069240, 126.2399288045637746, 15.00000000000006928 ) ) ;
#4993 = FACE_OUTER_BOUND ( 'NONE', #15668, .T. ) ;
#4994 = VERTEX_POINT ( 'NONE', #11952 ) ;
#4995 = CYLINDRICAL_SURFACE ( 'NONE', #5816, 4.000000000000024869 ) ;
#4996 = CARTESIAN_POINT ( 'NONE',  ( 124.5381772159375942, -151.5628872026272802, 36.00000000000000711 ) ) ;
#4997 = ORIENTED_EDGE ( 'NONE', *, *, #5154, .T. ) ;
#4998 = ADVANCED_FACE ( 'NONE', ( #17374, #10371 ), #3173, .T. ) ;
#4999 = VERTEX_POINT ( 'NONE', #9158 ) ;
#5000 = AXIS2_PLACEMENT_3D ( 'NONE', #11984, #9098, #16285 ) ;
#5001 = CARTESIAN_POINT ( 'NONE',  ( 5.233202738124664855, -19.34983604512936495, 54.79921157549230770 ) ) ;
#5002 = DIRECTION ( 'NONE',  ( 0.000000000000000000, 0.000000000000000000, 1.000000000000000000 ) ) ;
#5003 = ORIENTED_EDGE ( 'NONE', *, *, #2657, .T. ) ;
#5004 = DIRECTION ( 'NONE',  ( 1.000000000000000000, 0.000000000000000000, 0.000000000000000000 ) ) ;
#5005 =( NAMED_UNIT ( * ) PLANE_ANGLE_UNIT ( ) SI_UNIT ( $, .RADIAN. ) );
#5006 = LINE ( 'NONE', #12045, #17126 ) ;
#5007 = CARTESIAN_POINT ( 'NONE',  ( -68.99615306438106188, 36.56753083813027416, -15.00000000000001421 ) ) ;
#5008 = ORIENTED_EDGE ( 'NONE', *, *, #9621, .F. ) ;
#5009 = EDGE_CURVE ( 'NONE', #17707, #3371, #1678, .T. ) ;
#5010 = EDGE_CURVE ( 'NONE', #13442, #17304, #13763, .T. ) ;
#5011 = CARTESIAN_POINT ( 'NONE',  ( -67.79562744116532258, 82.83016482797231106, -167.1454815528550739 ) ) ;
#5012 = DIRECTION ( 'NONE',  ( 1.000000000000000000, 0.000000000000000000, 0.000000000000000000 ) ) ;
#5013 = DIRECTION ( 'NONE',  ( 0.000000000000000000, 0.000000000000000000, 1.000000000000000000 ) ) ;
#5014 = CARTESIAN_POINT ( 'NONE',  ( 15.23320273812466574, -111.0842361345572158, 57.00000000000000000 ) ) ;
#5015 = ORIENTED_EDGE ( 'NONE', *, *, #11477, .T. ) ;
#5016 = LINE ( 'NONE', #10936, #11786 ) ;
#5017 = PLANE ( 'NONE',  #7790 ) ;
#5018 = VERTEX_POINT ( 'NONE', #1759 ) ;
#5019 = DIRECTION ( 'NONE',  ( 0.000000000000000000, 0.000000000000000000, 1.000000000000000000 ) ) ;
#5020 = EDGE_CURVE ( 'NONE', #17887, #12880, #307, .T. ) ;
#5021 = CARTESIAN_POINT ( 'NONE',  ( -36.89438688693570612, 78.27883601870421160, 67.07281572422797922 ) ) ;
#5022 = ORIENTED_EDGE ( 'NONE', *, *, #15806, .F. ) ;
#5023 = EDGE_CURVE ( 'NONE', #2884, #703, #10764, .T. ) ;
#5024 = ORIENTED_EDGE ( 'NONE', *, *, #13214, .F. ) ;
#5025 = EDGE_CURVE ( 'NONE', #12950, #10713, #11863, .T. ) ;
#5026 = ADVANCED_FACE ( 'NONE', ( #8796 ), #4563, .T. ) ;
#5027 = AXIS2_PLACEMENT_3D ( 'NONE', #16455, #18157, #2332 ) ;
#5028 = DIRECTION ( 'NONE',  ( -1.000000000000000000, 0.000000000000000000, 0.000000000000000000 ) ) ;
#5029 = ORIENTED_EDGE ( 'NONE', *, *, #8501, .T. ) ;
#5030 = FACE_OUTER_BOUND ( 'NONE', #8067, .T. ) ;
#5031 = CARTESIAN_POINT ( 'NONE',  ( -70.64145177051501889, 58.17045213671937631, 22.35917033480641791 ) ) ;
#5032 = DIRECTION ( 'NONE',  ( -0.9396926207859157554, 0.3420201433256481738, -4.890320548438487362E-16 ) ) ;
#5033 = EDGE_CURVE ( 'NONE', #3439, #16762, #8884, .T. ) ;
#5034 = EDGE_CURVE ( 'NONE', #9243, #2078, #5695, .T. ) ;
#5035 = CARTESIAN_POINT ( 'NONE',  ( -57.08002265617300708, 84.22855780814606419, -35.00000000000000000 ) ) ;
#5036 = ADVANCED_FACE ( 'NONE', ( #4735 ), #9336, .F. ) ;
#5037 = CARTESIAN_POINT ( 'NONE',  ( -71.24615306438079188, 112.7846874652292399, -15.00000000000001421 ) ) ;
#5038 = CARTESIAN_POINT ( 'NONE',  ( -71.24615306438086293, 87.65194626522927024, 15.00000000000006928 ) ) ;
#5039 = EDGE_LOOP ( 'NONE', ( #11130, #4687, #15225, #3802, #10640, #1606, #18307, #12488 ) ) ;
#5040 = CARTESIAN_POINT ( 'NONE',  ( -72.62084357432196668, 59.30745156523346395, -22.61749258835635246 ) ) ;
#5041 = CARTESIAN_POINT ( 'NONE',  ( -68.99615306438082030, 86.83301323813022066, 15.00000000000006928 ) ) ;
#5042 = VECTOR ( 'NONE', #1915, 1000.000000000000114 ) ;
#5043 = ORIENTED_EDGE ( 'NONE', *, *, #3310, .T. ) ;
#5044 = CARTESIAN_POINT ( 'NONE',  ( -97.59262256747318531, 0.3328663868096687350, -25.00000000000000000 ) ) ;
#5045 = DIRECTION ( 'NONE',  ( 0.000000000000000000, 1.000000000000000000, 0.000000000000000000 ) ) ;
#5046 = EDGE_LOOP ( 'NONE', ( #4151, #5098, #16028, #15742 ) ) ;
#5047 = EDGE_CURVE ( 'NONE', #18453, #7572, #3815, .T. ) ;
#5048 = EDGE_CURVE ( 'NONE', #10428, #13041, #8112, .T. ) ;
#5049 = ORIENTED_EDGE ( 'NONE', *, *, #6856, .F. ) ;
#5050 = DIRECTION ( 'NONE',  ( -1.000000000000000000, 0.000000000000000000, 0.000000000000000000 ) ) ;
#5051 = DIRECTION ( 'NONE',  ( 0.000000000000000000, 0.000000000000000000, 1.000000000000000000 ) ) ;
#5052 = AXIS2_PLACEMENT_3D ( 'NONE', #6470, #17518, #16027 ) ;
#5053 = CARTESIAN_POINT ( 'NONE',  ( -41.66054475863654716, 53.50644796006596948, -24.87164372060468764 ) ) ;
#5054 = DIRECTION ( 'NONE',  ( 1.000000000000000000, 0.000000000000000000, 0.000000000000000000 ) ) ;
#5055 = ORIENTED_EDGE ( 'NONE', *, *, #2552, .T. ) ;
#5056 = CARTESIAN_POINT ( 'NONE',  ( -123.4618227840623632, -151.5628872026273086, 18.23991632971911514 ) ) ;
#5057 = VECTOR ( 'NONE', #7051, 1000.000000000000000 ) ;
#5058 = PLANE ( 'NONE',  #10810 ) ;
#5059 = ORIENTED_EDGE ( 'NONE', *, *, #4838, .T. ) ;
#5060 = CARTESIAN_POINT ( 'NONE',  ( -68.99615306438096241, 58.55867938813025120, -15.00000000000001421 ) ) ;
#5061 = LINE ( 'NONE', #16379, #949 ) ;
#5062 = CARTESIAN_POINT ( 'NONE',  ( -78.12361985383353158, 84.47473112397163675, 55.00000000000002132 ) ) ;
#5063 = LINE ( 'NONE', #3766, #11447 ) ;
#5064 = VERTEX_POINT ( 'NONE', #826 ) ;
#5065 = CARTESIAN_POINT ( 'NONE',  ( -123.4618227840623632, 84.22855780814606419, 55.00000000000001421 ) ) ;
#5066 = EDGE_LOOP ( 'NONE', ( #5354, #2926, #7190, #10376 ) ) ;
#5067 = CARTESIAN_POINT ( 'NONE',  ( -68.99615306438117557, 4.536748481662661092, 15.00000000000006928 ) ) ;
#5068 = VERTEX_POINT ( 'NONE', #15031 ) ;
#5069 = AXIS2_PLACEMENT_3D ( 'NONE', #287, #7490, #5981 ) ;
#5070 = AXIS2_PLACEMENT_3D ( 'NONE', #4301, #12542, #6734 ) ;
#5071 = ORIENTED_EDGE ( 'NONE', *, *, #15206, .F. ) ;
#5072 = CARTESIAN_POINT ( 'NONE',  ( -67.59262256747319952, 110.5691553257988460, 26.35917033480641436 ) ) ;
#5073 = DIRECTION ( 'NONE',  ( 0.000000000000000000, 0.000000000000000000, 1.000000000000000000 ) ) ;
#5074 = ORIENTED_EDGE ( 'NONE', *, *, #2628, .F. ) ;
#5075 = VECTOR ( 'NONE', #12906, 1000.000000000000000 ) ;
#5076 = CARTESIAN_POINT ( 'NONE',  ( -64.89435165812551531, 90.86016871721213306, 15.00000000000006928 ) ) ;
#5077 = CIRCLE ( 'NONE', #16736, 5.000000000000000000 ) ;
#5078 = CARTESIAN_POINT ( 'NONE',  ( -68.99615306438072082, 139.6252324316626812, 15.00000000000006928 ) ) ;
#5079 = ORIENTED_EDGE ( 'NONE', *, *, #2544, .T. ) ;
#5080 = CARTESIAN_POINT ( 'NONE',  ( 5.233202738124664855, -111.0842361345572158, 57.00000000000000000 ) ) ;
#5081 = AXIS2_PLACEMENT_3D ( 'NONE', #11116, #15500, #11305 ) ;
#5082 = VERTEX_POINT ( 'NONE', #3727 ) ;
#5083 = CIRCLE ( 'NONE', #3588, 4.599999999999992539 ) ;
#5084 = DIRECTION ( 'NONE',  ( 1.156482317317869999E-16, 0.000000000000000000, 1.000000000000000000 ) ) ;
#5085 = CARTESIAN_POINT ( 'NONE',  ( -68.99615306438104767, 11.43478963813027249, 15.00000000000006928 ) ) ;
#5087 = ORIENTED_EDGE ( 'NONE', *, *, #6881, .T. ) ;
#5086 = ADVANCED_FACE ( 'NONE', ( #4940 ), #7835, .F. ) ;
#5088 = DIRECTION ( 'NONE',  ( -5.204170427930409450E-16, 0.000000000000000000, 1.000000000000000000 ) ) ;
#5089 = CIRCLE ( 'NONE', #16453, 3.999999999999989786 ) ;
#5090 = CARTESIAN_POINT ( 'NONE',  ( -83.12361985383351737, 84.22855780814606419, -47.49999999999999289 ) ) ;
#5091 = ORIENTED_EDGE ( 'NONE', *, *, #17173, .T. ) ;
#5092 = ORIENTED_EDGE ( 'NONE', *, *, #14103, .F. ) ;
#5093 = VECTOR ( 'NONE', #13797, 1000.000000000000000 ) ;
#5094 = VECTOR ( 'NONE', #7706, 1000.000000000000000 ) ;
#5095 = VERTEX_POINT ( 'NONE', #10829 ) ;
#5096 = CARTESIAN_POINT ( 'NONE',  ( -71.24615306438073503, 129.3815214545637104, -15.00000000000001421 ) ) ;
#5097 = PLANE ( 'NONE',  #14166 ) ;
#5098 = ORIENTED_EDGE ( 'NONE', *, *, #16344, .T. ) ;
#5099 = ORIENTED_EDGE ( 'NONE', *, *, #10087, .F. ) ;
#5100 =( NAMED_UNIT ( * ) PLANE_ANGLE_UNIT ( ) SI_UNIT ( $, .RADIAN. ) );
#5101 = DIRECTION ( 'NONE',  ( 0.000000000000000000, 0.000000000000000000, 1.000000000000000000 ) ) ;
#5102 = DIRECTION ( 'NONE',  ( -1.000000000000000000, 0.000000000000000000, 1.156482317317869999E-16 ) ) ;
#5103 = LINE ( 'NONE', #16417, #17146 ) ;
#5104 = ORIENTED_EDGE ( 'NONE', *, *, #16684, .F. ) ;
#5105 = AXIS2_PLACEMENT_3D ( 'NONE', #7674, #17493, #3465 ) ;
#5106 = CARTESIAN_POINT ( 'NONE',  ( -68.99615306438083451, 99.39938383813029077, -15.00000000000001421 ) ) ;
#5107 = DIRECTION ( 'NONE',  ( -5.204170427930409450E-16, 0.000000000000000000, 1.000000000000000000 ) ) ;
#5108 = DIRECTION ( 'NONE',  ( -0.9396926207859084279, 0.3420201433256686574, 1.086737899652989892E-16 ) ) ;
#5109 = CARTESIAN_POINT ( 'NONE',  ( -78.12361985383350316, 84.22855780814606419, -61.50000000000000000 ) ) ;
#5110 = ORIENTED_EDGE ( 'NONE', *, *, #18430, .F. ) ;
#5111 = VECTOR ( 'NONE', #9467, 1000.000000000000000 ) ;
#5112 = AXIS2_PLACEMENT_3D ( 'NONE', #5254, #10969, #8159 ) ;
#5113 = DIRECTION ( 'NONE',  ( 0.000000000000000000, 0.000000000000000000, 1.000000000000000000 ) ) ;
#5114 = CARTESIAN_POINT ( 'NONE',  ( -127.5926225674731711, 57.88796029049329661, 30.35917033480640370 ) ) ;
#5115 = EDGE_LOOP ( 'NONE', ( #77, #740, #9702, #4076 ) ) ;
#5116 = CARTESIAN_POINT ( 'NONE',  ( -47.15582643534892782, 86.78830982163900387, 15.00000000000006928 ) ) ;
#5117 = CARTESIAN_POINT ( 'NONE',  ( -37.06381404437335902, 77.72742355542473547, 66.27118709564553001 ) ) ;
#5118 = ORIENTED_EDGE ( 'NONE', *, *, #8798, .F. ) ;
#5119 = ORIENTED_EDGE ( 'NONE', *, *, #8429, .T. ) ;
#5120 = AXIS2_PLACEMENT_3D ( 'NONE', #11804, #3270, #6245 ) ;
#5121 = EDGE_CURVE ( 'NONE', #13353, #10960, #6615, .T. ) ;
#5122 = CARTESIAN_POINT ( 'NONE',  ( -35.03642545851250389, 84.22855780814606419, -47.50000000000000000 ) ) ;
#5123 = ORIENTED_EDGE ( 'NONE', *, *, #7525, .F. ) ;
#5124 = VECTOR ( 'NONE', #6299, 1000.000000000000114 ) ;
#5125 = AXIS2_PLACEMENT_3D ( 'NONE', #7052, #15543, #960 ) ;
#5126 = CARTESIAN_POINT ( 'NONE',  ( -67.26033723204500347, 83.04399200740374454, -15.00000000000001243 ) ) ;
#5127 = PLANE ( 'NONE',  #393 ) ;
#5128 = CARTESIAN_POINT ( 'NONE',  ( -66.06069454268705954, 57.36660113903539582, 25.00000000000000355 ) ) ;
#5129 = DIRECTION ( 'NONE',  ( 1.000000000000000000, 0.000000000000000000, 0.000000000000000000 ) ) ;
#5130 = DIRECTION ( 'NONE',  ( 0.9396926207859158664, 0.3420201433256481738, 0.000000000000000000 ) ) ;
#5131 = CARTESIAN_POINT ( 'NONE',  ( -71.24615306438097662, 57.12489050456376560, -167.1454815528550739 ) ) ;
#5132 = VERTEX_POINT ( 'NONE', #2310 ) ;
#5133 = EDGE_CURVE ( 'NONE', #5248, #7744, #18254, .T. ) ;
#5134 = ADVANCED_FACE ( 'NONE', ( #12531 ), #12339, .T. ) ;
#5135 = AXIS2_PLACEMENT_3D ( 'NONE', #3589, #1923, #7532 ) ;
#5136 = CARTESIAN_POINT ( 'NONE',  ( -68.99615306438100504, 49.13390143813029454, 15.00000000000006928 ) ) ;
#5137 = DIRECTION ( 'NONE',  ( -1.000000000000000000, -0.000000000000000000, -0.000000000000000000 ) ) ;
#5138 = ORIENTED_EDGE ( 'NONE', *, *, #11144, .T. ) ;
#5139 = AXIS2_PLACEMENT_3D ( 'NONE', #3654, #6548, #17967 ) ;
#5140 = CARTESIAN_POINT ( 'NONE',  ( -27.58560781757364211, -92.35432432510553724, -7.309979984196388614 ) ) ;
#5141 = AXIS2_PLACEMENT_3D ( 'NONE', #12651, #4031, #6924 ) ;
#5142 = DIRECTION ( 'NONE',  ( 0.000000000000000000, 1.000000000000000000, 0.000000000000000000 ) ) ;
#5143 = ORIENTED_EDGE ( 'NONE', *, *, #17480, .T. ) ;
#5144 = EDGE_LOOP ( 'NONE', ( #2002, #14809, #16228, #3071 ) ) ;
#5145 = ADVANCED_FACE ( 'NONE', ( #913 ), #5017, .T. ) ;
#5146 = EDGE_CURVE ( 'NONE', #13337, #12706, #6441, .T. ) ;
#5147 = ADVANCED_FACE ( 'NONE', ( #14928 ), #2129, .F. ) ;
#5148 = ORIENTED_EDGE ( 'NONE', *, *, #15790, .F. ) ;
#5149 = EDGE_CURVE ( 'NONE', #14649, #3187, #3021, .T. ) ;
#5150 = LINE ( 'NONE', #17682, #17554 ) ;
#5151 = CARTESIAN_POINT ( 'NONE',  ( -71.24615306438073503, 128.4926507152292459, -167.1454815528550739 ) ) ;
#5152 = DIRECTION ( 'NONE',  ( 0.9396926207859158664, 0.3420201433256481738, -1.086737899652998397E-16 ) ) ;
#5153 = FACE_OUTER_BOUND ( 'NONE', #3397, .T. ) ;
#5154 = EDGE_CURVE ( 'NONE', #7063, #401, #14296, .T. ) ;
#5155 = CIRCLE ( 'NONE', #10837, 4.600000000000006750 ) ;
#5156 = DIRECTION ( 'NONE',  ( 0.9396926207859171987, 0.3420201433256445100, 4.890320548438495251E-16 ) ) ;
#5157 = CIRCLE ( 'NONE', #1299, 4.599999999999992539 ) ;
#5158 = CARTESIAN_POINT ( 'NONE',  ( -71.24615306438094819, 68.80239036522922902, -15.00000000000001421 ) ) ;
#5159 = VERTEX_POINT ( 'NONE', #4104 ) ;
#5160 = DIRECTION ( 'NONE',  ( 0.3420201433256612189, -0.9396926207859112035, 0.000000000000000000 ) ) ;
#5161 = FACE_OUTER_BOUND ( 'NONE', #6766, .T. ) ;
#5163 = VERTEX_POINT ( 'NONE', #16030 ) ;
#5162 = CARTESIAN_POINT ( 'NONE',  ( -68.99615306438100504, 42.85071613813029501, 15.00000000000006928 ) ) ;
#5164 = CARTESIAN_POINT ( 'NONE',  ( -112.3460510726627462, -91.53393135689864835, 8.561720054221641618 ) ) ;
#5165 = EDGE_CURVE ( 'NONE', #7640, #16893, #18229, .T. ) ;
#5166 = ADVANCED_FACE ( 'NONE', ( #5400 ), #11682, .T. ) ;
#5167 = CARTESIAN_POINT ( 'NONE',  ( -33.72855994630469212, 78.95224028009285178, 97.49999999999998579 ) ) ;
#5168 = VERTEX_POINT ( 'NONE', #8593 ) ;
#5169 = VECTOR ( 'NONE', #10270, 1000.000000000000000 ) ;
#5170 = CARTESIAN_POINT ( 'NONE',  ( -70.27900850916093134, -2.213358015103445098, -167.1454815528550739 ) ) ;
#5171 = ORIENTED_EDGE ( 'NONE', *, *, #16689, .T. ) ;
#5172 = EDGE_CURVE ( 'NONE', #13683, #10531, #2110, .T. ) ;
#5173 = AXIS2_PLACEMENT_3D ( 'NONE', #6126, #4385, #15792 ) ;
#5174 = VECTOR ( 'NONE', #2328, 1000.000000000000000 ) ;
#5175 = AXIS2_PLACEMENT_3D ( 'NONE', #8601, #2515, #9622 ) ;
#5176 = ORIENTED_EDGE ( 'NONE', *, *, #8626, .F. ) ;
#5177 = DIRECTION ( 'NONE',  ( -0.000000000000000000, -1.000000000000000000, -0.000000000000000000 ) ) ;
#5178 = LINE ( 'NONE', #1359, #6995 ) ;
#5179 = CARTESIAN_POINT ( 'NONE',  ( -71.24615306438114715, 15.39531531522927921, 15.00000000000006928 ) ) ;
#5180 = ORIENTED_EDGE ( 'NONE', *, *, #105, .F. ) ;
#5181 = APPLICATION_PROTOCOL_DEFINITION ( 'draft international standard', 'automotive_design', 1998, #13873 ) ;
#5182 = CARTESIAN_POINT ( 'NONE',  ( -107.5926225674731711, 57.88796029049330372, 30.38417033480641294 ) ) ;
#5183 = CARTESIAN_POINT ( 'NONE',  ( -67.59262256747315689, 0.000000000000000000, 0.000000000000000000 ) ) ;
#5184 = ORIENTED_EDGE ( 'NONE', *, *, #4449, .F. ) ;
#5185 = FACE_OUTER_BOUND ( 'NONE', #254, .T. ) ;
#5186 = DIRECTION ( 'NONE',  ( -0.9396926207859022107, 0.3420201433256853663, 1.086737899652982620E-16 ) ) ;
#5187 = AXIS2_PLACEMENT_3D ( 'NONE', #6310, #12322, #17740 ) ;
#5188 = ORIENTED_EDGE ( 'NONE', *, *, #4232, .T. ) ;
#5189 = AXIS2_PLACEMENT_3D ( 'NONE', #4154, #9861, #16870 ) ;
#5190 = CARTESIAN_POINT ( 'NONE',  ( -76.09664428591263174, 106.6093187847199459, -26.96894390707464240 ) ) ;
#5191 = LINE ( 'NONE', #5085, #5124 ) ;
#5192 = ORIENTED_EDGE ( 'NONE', *, *, #11778, .F. ) ;
#5193 = DIRECTION ( 'NONE',  ( 0.000000000000000000, 0.000000000000000000, 1.000000000000000000 ) ) ;
#5194 = CARTESIAN_POINT ( 'NONE',  ( -68.99615306438097662, 58.55867938813025830, -167.1454815528550739 ) ) ;
#5195 = VERTEX_POINT ( 'NONE', #74 ) ;
#5196 = AXIS2_PLACEMENT_3D ( 'NONE', #2710, #2619, #15797 ) ;
#5197 = VECTOR ( 'NONE', #17150, 1000.000000000000114 ) ;
#5198 = ORIENTED_EDGE ( 'NONE', *, *, #6041, .F. ) ;
#5199 = DIRECTION ( 'NONE',  ( 1.000000000000000000, 0.000000000000000000, 0.000000000000000000 ) ) ;
#5200 = CARTESIAN_POINT ( 'NONE',  ( -71.24615306438111872, 22.56737135456379661, -167.1454815528550739 ) ) ;
#5201 = PLANE ( 'NONE',  #11394 ) ;
#5202 = CARTESIAN_POINT ( 'NONE',  ( -76.74183620129869610, 76.72881973191590532, 62.99780471344396204 ) ) ;
#5203 = LINE ( 'NONE', #15022, #1595 ) ;
#5204 = CYLINDRICAL_SURFACE ( 'NONE', #18362, 170.8515291679562154 ) ;
#5205 = ORIENTED_EDGE ( 'NONE', *, *, #12596, .T. ) ;
#5206 = VECTOR ( 'NONE', #17411, 1000.000000000000114 ) ;
#5207 = EDGE_CURVE ( 'NONE', #10207, #16011, #11733, .T. ) ;
#5208 = CARTESIAN_POINT ( 'NONE',  ( -71.24615306438111872, 19.42577870456376132, 15.00000000000006928 ) ) ;
#5209 = CARTESIAN_POINT ( 'NONE',  ( -71.24615306438116136, 3.717815454563756727, -15.00000000000001421 ) ) ;
#5210 = DIRECTION ( 'NONE',  ( 0.000000000000000000, 0.000000000000000000, -1.000000000000000000 ) ) ;
#5211 = DIRECTION ( 'NONE',  ( 0.000000000000000000, 0.000000000000000000, 1.000000000000000000 ) ) ;
#5212 = CARTESIAN_POINT ( 'NONE',  ( -65.06546592763127990, -111.0842361345572158, -2.621725226070001387E-13 ) ) ;
#5213 = ORIENTED_EDGE ( 'NONE', *, *, #1402, .F. ) ;
#5214 = VECTOR ( 'NONE', #15008, 1000.000000000000000 ) ;
#5215 = AXIS2_PLACEMENT_3D ( 'NONE', #17065, #2580, #15573 ) ;
#5216 = AXIS2_PLACEMENT_3D ( 'NONE', #7048, #14049, #12664 ) ;
#5217 = LINE ( 'NONE', #4835, #14193 ) ;
#5218 = DIRECTION ( 'NONE',  ( 0.000000000000000000, 0.000000000000000000, -1.000000000000000000 ) ) ;
#5219 = ORIENTED_EDGE ( 'NONE', *, *, #4121, .F. ) ;
#5220 = DIRECTION ( 'NONE',  ( -0.9396926207859103153, 0.3420201433256635504, 0.000000000000000000 ) ) ;
#5221 = PRESENTATION_STYLE_ASSIGNMENT (( #15427 ) ) ;
#5222 = ORIENTED_EDGE ( 'NONE', *, *, #15349, .T. ) ;
#5223 = ORIENTED_EDGE ( 'NONE', *, *, #8129, .T. ) ;
#5224 = DIRECTION ( 'NONE',  ( -1.000000000000000000, -0.000000000000000000, -6.950654929607132427E-15 ) ) ;
#5225 = ORIENTED_EDGE ( 'NONE', *, *, #10037, .T. ) ;
#5226 = AXIS2_PLACEMENT_3D ( 'NONE', #9533, #15050, #3922 ) ;
#5227 = AXIS2_PLACEMENT_3D ( 'NONE', #16051, #3241, #8960 ) ;
#5228 = LINE ( 'NONE', #18342, #3436 ) ;
#5229 = DIRECTION ( 'NONE',  ( 0.000000000000000000, 1.000000000000000000, 0.000000000000000000 ) ) ;
#5230 = CARTESIAN_POINT ( 'NONE',  ( 5.699999999999996625, 0.000000000000000000, 0.000000000000000000 ) ) ;
#5231 = LINE ( 'NONE', #10950, #13455 ) ;
#5232 = DIRECTION ( 'NONE',  ( 1.000000000000000000, 0.000000000000000000, 0.000000000000000000 ) ) ;
#5233 = CYLINDRICAL_SURFACE ( 'NONE', #13597, 26.04359719766049253 ) ;
#5234 = DIRECTION ( 'NONE',  ( 0.000000000000000000, 0.000000000000000000, -1.000000000000000000 ) ) ;
#5235 = EDGE_LOOP ( 'NONE', ( #5301, #4701, #11050, #5833 ) ) ;
#5236 = EDGE_CURVE ( 'NONE', #11287, #9128, #17425, .T. ) ;
#5237 = DIRECTION ( 'NONE',  ( -1.000000000000000000, -3.016910393003142859E-15, 0.000000000000000000 ) ) ;
#5238 = FACE_OUTER_BOUND ( 'NONE', #1995, .T. ) ;
#5239 = ORIENTED_EDGE ( 'NONE', *, *, #10507, .F. ) ;
#5240 = LINE ( 'NONE', #13574, #12111 ) ;
#5241 = CIRCLE ( 'NONE', #18404, 10.38004356723770627 ) ;
#5242 = DIRECTION ( 'NONE',  ( 1.000000000000000000, -0.000000000000000000, -0.000000000000000000 ) ) ;
#5244 = ORIENTED_EDGE ( 'NONE', *, *, #6145, .T. ) ;
#5243 = AXIS2_PLACEMENT_3D ( 'NONE', #12624, #16521, #9511 ) ;
#5245 = ADVANCED_BREP_SHAPE_REPRESENTATION ( '', ( #257, #16217 ), #8171 ) ;
#5246 = VERTEX_POINT ( 'NONE', #5677 ) ;
#5247 = EDGE_CURVE ( 'NONE', #9018, #10635, #1396, .T. ) ;
#5248 = VERTEX_POINT ( 'NONE', #7098 ) ;
#5249 = DIRECTION ( 'NONE',  ( 0.3420201433256444545, -0.9396926207859171987, 0.000000000000000000 ) ) ;
#5250 = LINE ( 'NONE', #3756, #13820 ) ;
#5251 = PLANE ( 'NONE',  #16543 ) ;
#5252 = PLANE ( 'NONE',  #1886 ) ;
#5253 = CARTESIAN_POINT ( 'NONE',  ( -68.99615306438072082, 133.9569029881302811, -167.1454815528550739 ) ) ;
#5254 = CARTESIAN_POINT ( 'NONE',  ( -107.5676225674731938, 110.5691553257988460, -26.35917033480641436 ) ) ;
#5255 = ORIENTED_EDGE ( 'NONE', *, *, #16936, .F. ) ;
#5256 = ADVANCED_FACE ( 'NONE', ( #1807 ), #4005, .T. ) ;
#5257 = CARTESIAN_POINT ( 'NONE',  ( -92.59262256747319952, 57.88796029049329661, 22.35917033480642502 ) ) ;
#5258 = DIRECTION ( 'NONE',  ( 0.000000000000000000, 1.000000000000000000, 0.000000000000000000 ) ) ;
#5260 = ORIENTED_EDGE ( 'NONE', *, *, #803, .F. ) ;
#5259 = DIRECTION ( 'NONE',  ( 0.000000000000000000, 0.000000000000000000, 1.000000000000000000 ) ) ;
#5261 = EDGE_CURVE ( 'NONE', #9843, #13900, #4290, .T. ) ;
#5262 = CARTESIAN_POINT ( 'NONE',  ( -68.99615306438080609, 105.0677132816627051, -15.00000000000001421 ) ) ;
#5263 = CARTESIAN_POINT ( 'NONE',  ( -46.71322837820016360, 91.21279551874765446, -167.1454815528550739 ) ) ;
#5264 = EDGE_LOOP ( 'NONE', ( #13325, #17454, #6782, #8580 ) ) ;
#5265 = ADVANCED_FACE ( 'NONE', ( #8925 ), #12807, .T. ) ;
#5266 = FACE_OUTER_BOUND ( 'NONE', #3404, .T. ) ;
#5267 = ORIENTED_EDGE ( 'NONE', *, *, #815, .F. ) ;
#5268 = EDGE_CURVE ( 'NONE', #5064, #16126, #9808, .T. ) ;
#5269 = ADVANCED_FACE ( 'NONE', ( #2891 ), #15508, .T. ) ;
#5270 = ORIENTED_EDGE ( 'NONE', *, *, #15349, .F. ) ;
#5271 = EDGE_CURVE ( 'NONE', #8070, #1253, #5588, .T. ) ;
#5272 = CARTESIAN_POINT ( 'NONE',  ( -97.59262256747319952, 114.3311569208253786, 25.00000000000000000 ) ) ;
#5273 = EDGE_CURVE ( 'NONE', #10920, #13449, #12197, .T. ) ;
#5274 = FACE_OUTER_BOUND ( 'NONE', #12522, .T. ) ;
#5275 = DIRECTION ( 'NONE',  ( 0.9396926207859102043, 0.3420201433256637724, -1.086737899652991864E-16 ) ) ;
#5276 = ORIENTED_EDGE ( 'NONE', *, *, #5994, .T. ) ;
#5277 = CARTESIAN_POINT ( 'NONE',  ( -31.40585197410439378, -91.08930925317537231, 10.39386867823088068 ) ) ;
#5278 = LINE ( 'NONE', #13794, #6095 ) ;
#5279 = EDGE_LOOP ( 'NONE', ( #16180, #5447, #10584, #9122 ) ) ;
#5280 = EDGE_CURVE ( 'NONE', #14482, #14175, #17268, .T. ) ;
#5281 = CARTESIAN_POINT ( 'NONE',  ( -71.24615306438103346, 46.81124181522922356, -15.00000000000001421 ) ) ;
#5282 = PLANE ( 'NONE',  #12290 ) ;
#5283 = EDGE_CURVE ( 'NONE', #8741, #4662, #4190, .T. ) ;
#5284 = CYLINDRICAL_SURFACE ( 'NONE', #1280, 4.599999999999992539 ) ;
#5285 = EDGE_LOOP ( 'NONE', ( #6716, #7854, #10820, #3707 ) ) ;
#5286 = DIRECTION ( 'NONE',  ( 0.000000000000000000, 0.000000000000000000, -1.000000000000000000 ) ) ;
#5287 = FACE_OUTER_BOUND ( 'NONE', #1156, .T. ) ;
#5288 = EDGE_LOOP ( 'NONE', ( #7629, #16532, #9236, #6598 ) ) ;
#5289 = DIRECTION ( 'NONE',  ( 1.000000000000000000, 0.000000000000000000, 0.000000000000000000 ) ) ;
#5290 = FACE_OUTER_BOUND ( 'NONE', #3504, .T. ) ;
#5291 = EDGE_LOOP ( 'NONE', ( #17605, #18491, #13193, #4916 ) ) ;
#5292 = VERTEX_POINT ( 'NONE', #9903 ) ;
#5293 = EDGE_CURVE ( 'NONE', #1839, #9751, #15612, .T. ) ;
#5294 = DIRECTION ( 'NONE',  ( -0.000000000000000000, -0.000000000000000000, 1.000000000000000000 ) ) ;
#5295 = FACE_OUTER_BOUND ( 'NONE', #5285, .T. ) ;
#5296 = ORIENTED_EDGE ( 'NONE', *, *, #11667, .F. ) ;
#5297 = CARTESIAN_POINT ( 'NONE',  ( -65.17806329749801364, 93.75072866207683830, -167.1454815528550739 ) ) ;
#5298 = CARTESIAN_POINT ( 'NONE',  ( -68.99615306438106188, 35.95267498166268894, -167.1454815528550739 ) ) ;
#5299 = LINE ( 'NONE', #10927, #10554 ) ;
#5300 = CARTESIAN_POINT ( 'NONE',  ( -71.24615306438120399, -0.3126479347707321610, -167.1454815528550739 ) ) ;
#5301 = ORIENTED_EDGE ( 'NONE', *, *, #7319, .F. ) ;
#5302 = FACE_OUTER_BOUND ( 'NONE', #12758, .T. ) ;
#5303 = DIRECTION ( 'NONE',  ( 0.000000000000000000, 0.000000000000000000, 1.000000000000000000 ) ) ;
#5304 = CARTESIAN_POINT ( 'NONE',  ( -68.99615306438087714, 80.54982793813027797, -15.00000000000001421 ) ) ;
#5305 = DIRECTION ( 'NONE',  ( 0.000000000000000000, 0.000000000000000000, 1.000000000000000000 ) ) ;
#5306 = DIRECTION ( 'NONE',  ( -1.000000000000000000, -1.119176436114069332E-16, 0.000000000000000000 ) ) ;
#5307 = VERTEX_POINT ( 'NONE', #7887 ) ;
#5308 = CARTESIAN_POINT ( 'NONE',  ( -71.24615306438080609, 103.3599095152292193, 15.00000000000006928 ) ) ;
#5309 = DIRECTION ( 'NONE',  ( 1.000000000000000000, 0.000000000000000000, 0.000000000000000000 ) ) ;
#5310 = DIRECTION ( 'NONE',  ( 0.000000000000000000, 0.000000000000000000, -1.000000000000000000 ) ) ;
#5311 = ORIENTED_EDGE ( 'NONE', *, *, #12953, .F. ) ;
#5312 = ORIENTED_EDGE ( 'NONE', *, *, #17681, .T. ) ;
#5313 = ORIENTED_EDGE ( 'NONE', *, *, #8487, .T. ) ;
#5314 = DIRECTION ( 'NONE',  ( 0.000000000000000000, -5.551115123125747573E-17, -1.000000000000000000 ) ) ;
#5315 = DIRECTION ( 'NONE',  ( 0.000000000000000000, 0.000000000000000000, 1.000000000000000000 ) ) ;
#5316 = DIRECTION ( 'NONE',  ( 0.000000000000000000, -1.000000000000000000, 5.551115123125748189E-17 ) ) ;
#5317 = LINE ( 'NONE', #14132, #13754 ) ;
#5318 = CARTESIAN_POINT ( 'NONE',  ( -8.273817828780008867E-15, 5.788408252967876422, 2.974182810908626351 ) ) ;
#5319 = CARTESIAN_POINT ( 'NONE',  ( -47.50120849787443689, 51.11741075767032783, 26.54703875325328966 ) ) ;
#5320 = DIRECTION ( 'NONE',  ( 0.000000000000000000, 0.000000000000000000, 1.000000000000000000 ) ) ;
#5321 = ORIENTED_EDGE ( 'NONE', *, *, #9877, .F. ) ;
#5322 = DIRECTION ( 'NONE',  ( -5.204170427930409450E-16, 0.000000000000000000, 1.000000000000000000 ) ) ;
#5323 = LINE ( 'NONE', #15146, #1803 ) ;
#5324 = ORIENTED_EDGE ( 'NONE', *, *, #5382, .F. ) ;
#5325 = ADVANCED_FACE ( 'NONE', ( #14806 ), #9387, .F. ) ;
#5326 = LINE ( 'NONE', #6452, #4929 ) ;
#5327 = DIRECTION ( 'NONE',  ( 1.156482317317869999E-16, 0.000000000000000000, 1.000000000000000000 ) ) ;
#5328 = ORIENTED_EDGE ( 'NONE', *, *, #2403, .F. ) ;
#5329 = VECTOR ( 'NONE', #12929, 1000.000000000000000 ) ;
#5330 = VERTEX_POINT ( 'NONE', #6472 ) ;
#5331 = EDGE_LOOP ( 'NONE', ( #17776, #11304, #13543, #5655 ) ) ;
#5332 = CARTESIAN_POINT ( 'NONE',  ( -76.37409655828280108, -96.08423613455721579, 45.05044770573179846 ) ) ;
#5333 = DIRECTION ( 'NONE',  ( 0.000000000000000000, 1.000000000000000000, -0.000000000000000000 ) ) ;
#5334 = CARTESIAN_POINT ( 'NONE',  ( -71.24615306438114715, 13.14259340456377956, 15.00000000000006928 ) ) ;
#5335 = DIRECTION ( 'NONE',  ( 0.3420201433256612189, -0.9396926207859112035, 0.000000000000000000 ) ) ;
#5336 = CARTESIAN_POINT ( 'NONE',  ( -68.99615306438083451, 95.64293533166268446, 15.00000000000006928 ) ) ;
#5337 = VERTEX_POINT ( 'NONE', #6377 ) ;
#5338 = CIRCLE ( 'NONE', #1766, 4.599999999999999645 ) ;
#5339 = LINE ( 'NONE', #5060, #12910 ) ;
#5340 = CARTESIAN_POINT ( 'NONE',  ( -64.18632899337946185, 107.0896764944433954, 97.49999999999998579 ) ) ;
#5342 = VERTEX_POINT ( 'NONE', #3574 ) ;
#5341 = CARTESIAN_POINT ( 'NONE',  ( -77.02089413874927004, 90.95236025322215312, 65.83173792382639533 ) ) ;
#5343 = CARTESIAN_POINT ( 'NONE',  ( 0.5805565836007609004, 7.505553499465141165, -1.387778780781445676E-14 ) ) ;
#5344 = LINE ( 'NONE', #865, #590 ) ;
#5345 = ORIENTED_EDGE ( 'NONE', *, *, #8614, .F. ) ;
#5346 = EDGE_CURVE ( 'NONE', #7186, #773, #6280, .T. ) ;
#5347 = FACE_OUTER_BOUND ( 'NONE', #4304, .T. ) ;
#5348 = VERTEX_POINT ( 'NONE', #5067 ) ;
#5349 = AXIS2_PLACEMENT_3D ( 'NONE', #12699, #16681, #3875 ) ;
#5350 = ORIENTED_EDGE ( 'NONE', *, *, #10087, .T. ) ;
#5351 = EDGE_CURVE ( 'NONE', #4300, #15197, #14004, .T. ) ;
#5352 = CARTESIAN_POINT ( 'NONE',  ( -53.44605150580733266, 72.26844686893191749, 15.00000000000006928 ) ) ;
#5353 = CARTESIAN_POINT ( 'NONE',  ( -60.06546592763088910, -91.08423613455721579, -38.97384619189688948 ) ) ;
#5354 = ORIENTED_EDGE ( 'NONE', *, *, #16926, .T. ) ;
#5355 = SHAPE_DEFINITION_REPRESENTATION ( #11205, #5501 ) ;
#5356 = CARTESIAN_POINT ( 'NONE',  ( 5.090901028739964751, 20.32480939964089117, -43.45823631389497876 ) ) ;
#5357 = CARTESIAN_POINT ( 'NONE',  ( -57.08002265617301418, 106.1506877598988154, 97.49999999999998579 ) ) ;
#5358 = ORIENTED_EDGE ( 'NONE', *, *, #6020, .F. ) ;
#5359 = DIRECTION ( 'NONE',  ( 1.000000000000000000, 0.000000000000000000, 0.000000000000000000 ) ) ;
#5360 = CARTESIAN_POINT ( 'NONE',  ( -68.99615306438089135, 79.93497208166267853, -15.00000000000001421 ) ) ;
#5361 = ADVANCED_FACE ( 'NONE', ( #502 ), #17601, .T. ) ;
#5362 = ORIENTED_EDGE ( 'NONE', *, *, #10485, .T. ) ;
#5364 = EDGE_CURVE ( 'NONE', #15862, #8464, #13602, .T. ) ;
#5363 = VECTOR ( 'NONE', #4497, 1000.000000000000000 ) ;
#5365 = CARTESIAN_POINT ( 'NONE',  ( -55.10846673861666289, 96.57209730311868157, 15.00000000000006928 ) ) ;
#5366 = DIRECTION ( 'NONE',  ( 1.000000000000000000, 0.000000000000000000, 3.771137991253917233E-16 ) ) ;
#5367 = EDGE_LOOP ( 'NONE', ( #14926, #1137, #2014, #16275 ) ) ;
#5368 = ADVANCED_FACE ( 'NONE', ( #14987 ), #1996, .F. ) ;
#5369 = VECTOR ( 'NONE', #11057, 1000.000000000000000 ) ;
#5370 = PLANE ( 'NONE',  #8821 ) ;
#5371 = LINE ( 'NONE', #18403, #15375 ) ;
#5372 = ORIENTED_EDGE ( 'NONE', *, *, #13609, .T. ) ;
#5373 = ORIENTED_EDGE ( 'NONE', *, *, #6981, .T. ) ;
#5374 = ADVANCED_FACE ( 'NONE', ( #411 ), #2088, .T. ) ;
#5375 = EDGE_CURVE ( 'NONE', #1161, #13022, #17883, .T. ) ;
#5376 = EDGE_CURVE ( 'NONE', #8500, #9465, #4785, .T. ) ;
#5377 = ORIENTED_EDGE ( 'NONE', *, *, #11559, .T. ) ;
#5378 = CIRCLE ( 'NONE', #8697, 4.599999999999999645 ) ;
#5379 = DIRECTION ( 'NONE',  ( -0.000000000000000000, 1.000000000000000000, -0.000000000000000000 ) ) ;
#5380 = CARTESIAN_POINT ( 'NONE',  ( -64.09025127992791226, 117.8748711238780373, -35.00000000000000000 ) ) ;
#5381 = ORIENTED_EDGE ( 'NONE', *, *, #13065, .F. ) ;
#5382 = EDGE_CURVE ( 'NONE', #17521, #15122, #10502, .T. ) ;
#5383 = CIRCLE ( 'NONE', #4491, 11.04359719766049430 ) ;
#5384 = CARTESIAN_POINT ( 'NONE',  ( -71.24615306438113294, 0.5762228045638172480, 15.00000000000006928 ) ) ;
#5385 = DIRECTION ( 'NONE',  ( 0.000000000000000000, 0.000000000000000000, 1.000000000000000000 ) ) ;
#5386 = AXIS2_PLACEMENT_3D ( 'NONE', #16916, #4105, #12903 ) ;
#5387 = CARTESIAN_POINT ( 'NONE',  ( -68.99615306438117557, 4.536748481662661092, -15.00000000000001421 ) ) ;
#5388 = DIRECTION ( 'NONE',  ( 1.000000000000000000, 0.000000000000000000, 0.000000000000000000 ) ) ;
#5389 = ORIENTED_EDGE ( 'NONE', *, *, #1507, .F. ) ;
#5390 = EDGE_CURVE ( 'NONE', #18482, #1708, #3389, .T. ) ;
#5391 = CARTESIAN_POINT ( 'NONE',  ( -68.99615306438116136, 5.151604338130299610, -15.00000000000001421 ) ) ;
#5392 = PLANE ( 'NONE',  #10932 ) ;
#5393 =( NAMED_UNIT ( * ) PLANE_ANGLE_UNIT ( ) SI_UNIT ( $, .RADIAN. ) );
#5394 = FACE_OUTER_BOUND ( 'NONE', #5886, .T. ) ;
#5395 = DIRECTION ( 'NONE',  ( 0.3420201433256686574, 0.9396926207859084279, -0.000000000000000000 ) ) ;
#5396 = ORIENTED_EDGE ( 'NONE', *, *, #3780, .F. ) ;
#5397 = CIRCLE ( 'NONE', #3592, 10.24900000000000055 ) ;
#5398 = ADVANCED_FACE ( 'NONE', ( #3677 ), #17520, .F. ) ;
#5399 = CARTESIAN_POINT ( 'NONE',  ( -68.99615306438106188, 29.66948968166269296, -167.1454815528550739 ) ) ;
#5400 = FACE_OUTER_BOUND ( 'NONE', #7718, .T. ) ;
#5401 = AXIS2_PLACEMENT_3D ( 'NONE', #2225, #3618, #7938 ) ;
#5402 = EDGE_CURVE ( 'NONE', #5649, #14470, #16103, .T. ) ;
#5403 = FACE_OUTER_BOUND ( 'NONE', #10010, .T. ) ;
#5404 = VECTOR ( 'NONE', #7648, 1000.000000000000114 ) ;
#5405 =( LENGTH_UNIT ( ) NAMED_UNIT ( * ) SI_UNIT ( .MILLI., .METRE. ) );
#5406 = ORIENTED_EDGE ( 'NONE', *, *, #17178, .F. ) ;
#5407 = EDGE_LOOP ( 'NONE', ( #14144, #12511, #2777, #2302, #7802, #9527, #13802, #17295, #9895, #8177, #14323, #7641 ) ) ;
#5408 = CARTESIAN_POINT ( 'NONE',  ( -68.99615306438080609, 105.6825691381303045, 15.00000000000006928 ) ) ;
#5409 = AXIS2_PLACEMENT_3D ( 'NONE', #15576, #11469, #15758 ) ;
#5410 = DIRECTION ( 'NONE',  ( -0.000000000000000000, -0.000000000000000000, -1.000000000000000000 ) ) ;
#5411 = DIRECTION ( 'NONE',  ( 0.000000000000000000, -0.5000000000000008882, -0.8660254037844381525 ) ) ;
#5412 = DIRECTION ( 'NONE',  ( 1.047634945911800068E-14, -0.000000000000000000, -1.000000000000000000 ) ) ;
#5413 = ORIENTED_EDGE ( 'NONE', *, *, #3312, .T. ) ;
#5414 = DIRECTION ( 'NONE',  ( -0.9396926207859084279, 0.3420201433256687684, 1.086737899652989769E-16 ) ) ;
#5415 = AXIS2_PLACEMENT_3D ( 'NONE', #2476, #9780, #3871 ) ;
#5416 = VECTOR ( 'NONE', #10598, 1000.000000000000114 ) ;
#5417 = CARTESIAN_POINT ( 'NONE',  ( -57.08002265617300708, 84.22855780814606419, -167.1454815528550739 ) ) ;
#5418 = CARTESIAN_POINT ( 'NONE',  ( -81.37409655828280108, -91.08423613455721579, 38.97384619189696764 ) ) ;
#5419 = ORIENTED_EDGE ( 'NONE', *, *, #12634, .T. ) ;
#5420 = DIRECTION ( 'NONE',  ( -0.000000000000000000, -1.000000000000000000, 0.000000000000000000 ) ) ;
#5421 = EDGE_LOOP ( 'NONE', ( #313, #6789, #18169, #8117 ) ) ;
#5422 = VECTOR ( 'NONE', #13680, 1000.000000000000000 ) ;
#5423 = CARTESIAN_POINT ( 'NONE',  ( -71.24615306438089135, 81.36876096522922808, 15.00000000000006928 ) ) ;
#5424 = CARTESIAN_POINT ( 'NONE',  ( -68.99615306438077766, 111.9657544381302330, -15.00000000000001421 ) ) ;
#5425 = VERTEX_POINT ( 'NONE', #12004 ) ;
#5426 = VERTEX_POINT ( 'NONE', #17702 ) ;
#5427 = AXIS2_PLACEMENT_3D ( 'NONE', #4972, #4880, #9378 ) ;
#5428 = AXIS2_PLACEMENT_3D ( 'NONE', #18263, #5437, #15459 ) ;
#5429 = EDGE_LOOP ( 'NONE', ( #2312, #14083, #16242, #3768 ) ) ;
#5430 = DIRECTION ( 'NONE',  ( -0.000000000000000000, -1.000000000000000000, -0.000000000000000000 ) ) ;
#5431 = CARTESIAN_POINT ( 'NONE',  ( -44.49764538373973721, 84.22855780814606419, 37.50000000000000000 ) ) ;
#5432 = DIRECTION ( 'NONE',  ( 1.000000000000000000, 0.000000000000000000, 0.000000000000000000 ) ) ;
#5433 = EDGE_CURVE ( 'NONE', #8708, #16262, #688, .T. ) ;
#5434 = DIRECTION ( 'NONE',  ( -0.000000000000000000, -0.000000000000000000, -1.000000000000000000 ) ) ;
#5435 = VECTOR ( 'NONE', #4535, 1000.000000000000114 ) ;
#5436 = LINE ( 'NONE', #5713, #2995 ) ;
#5437 = DIRECTION ( 'NONE',  ( -1.000000000000000000, -0.000000000000000000, -0.000000000000000000 ) ) ;
#5438 = EDGE_LOOP ( 'NONE', ( #17008, #17427, #15969, #10124 ) ) ;
#5439 = DIRECTION ( 'NONE',  ( -1.000000000000000000, 0.000000000000000000, 0.000000000000000000 ) ) ;
#5440 = DIRECTION ( 'NONE',  ( 0.000000000000000000, -4.000800291689476871E-17, -1.000000000000000000 ) ) ;
#5442 = ORIENTED_EDGE ( 'NONE', *, *, #17161, .F. ) ;
#5441 = DIRECTION ( 'NONE',  ( 0.000000000000000000, 0.000000000000000000, -1.000000000000000000 ) ) ;
#5443 = DIRECTION ( 'NONE',  ( 0.000000000000000000, 0.000000000000000000, 1.000000000000000000 ) ) ;
#5444 = CIRCLE ( 'NONE', #15898, 6.500000000000039968 ) ;
#5445 = VECTOR ( 'NONE', #17209, 1000.000000000000000 ) ;
#5446 = CARTESIAN_POINT ( 'NONE',  ( -71.24615306438073503, 128.4926507152292459, 15.00000000000006928 ) ) ;
#5447 = ORIENTED_EDGE ( 'NONE', *, *, #11701, .T. ) ;
#5448 = LINE ( 'NONE', #6770, #4716 ) ;
#5449 = ORIENTED_EDGE ( 'NONE', *, *, #4595, .T. ) ;
#5450 = VECTOR ( 'NONE', #14447, 1000.000000000000000 ) ;
#5451 = VERTEX_POINT ( 'NONE', #16302 ) ;
#5452 = AXIS2_PLACEMENT_3D ( 'NONE', #17783, #2257, #6360 ) ;
#5453 = CIRCLE ( 'NONE', #8459, 5.654315315325682434 ) ;
#5454 = DIRECTION ( 'NONE',  ( -0.000000000000000000, -0.000000000000000000, 1.000000000000000000 ) ) ;
#5455 = DIRECTION ( 'NONE',  ( 1.000000000000000000, 0.000000000000000000, 5.551115123125784674E-16 ) ) ;
#5456 = CARTESIAN_POINT ( 'NONE',  ( -57.08002265617300708, 84.22855780814606419, -167.1454815528550739 ) ) ;
#5457 = ORIENTED_EDGE ( 'NONE', *, *, #12856, .F. ) ;
#5458 = SHAPE_DEFINITION_REPRESENTATION ( #9535, #13055 ) ;
#5459 = ORIENTED_EDGE ( 'NONE', *, *, #15324, .T. ) ;
#5460 = CARTESIAN_POINT ( 'NONE',  ( 8.584122944725191218, 13.03299671059484233, -46.30665401617704902 ) ) ;
#5461 = DIRECTION ( 'NONE',  ( -0.000000000000000000, 1.000000000000000000, -0.000000000000000000 ) ) ;
#5462 = EDGE_LOOP ( 'NONE', ( #16423, #5593, #16168, #2411 ) ) ;
#5463 = VECTOR ( 'NONE', #3069, 1000.000000000000000 ) ;
#5464 = LINE ( 'NONE', #12305, #11402 ) ;
#5465 = CARTESIAN_POINT ( 'NONE',  ( -69.25984391241293281, 110.9679338156112323, 22.35917033480641791 ) ) ;
#5466 = CARTESIAN_POINT ( 'NONE',  ( -57.08002265617300708, 84.22855780814606419, -61.50000000000000000 ) ) ;
#5467 = ORIENTED_EDGE ( 'NONE', *, *, #18072, .F. ) ;
#5468 = CARTESIAN_POINT ( 'NONE',  ( -68.99615306438109030, 17.10311908166270456, -15.00000000000001421 ) ) ;
#5469 = CARTESIAN_POINT ( 'NONE',  ( -65.50906076758114693, 77.46608744949911340, 15.00000000000006928 ) ) ;
#5470 = VERTEX_POINT ( 'NONE', #3489 ) ;
#5471 = EDGE_CURVE ( 'NONE', #13044, #4868, #7796, .T. ) ;
#5472 = CIRCLE ( 'NONE', #3696, 20.99999999999998934 ) ;
#5473 = CARTESIAN_POINT ( 'NONE',  ( -68.99615306438100504, 45.99230878813026635, -167.1454815528550739 ) ) ;
#5474 = VECTOR ( 'NONE', #2136, 1000.000000000000000 ) ;
#5475 = DIRECTION ( 'NONE',  ( -0.9396926207859157554, 0.3420201433256481738, -4.890320548438487362E-16 ) ) ;
#5476 = ORIENTED_EDGE ( 'NONE', *, *, #8130, .T. ) ;
#5477 = ORIENTED_EDGE ( 'NONE', *, *, #1381, .F. ) ;
#5478 = ADVANCED_FACE ( 'NONE', ( #16865 ), #2334, .T. ) ;
#5479 = DIRECTION ( 'NONE',  ( 0.000000000000000000, 0.000000000000000000, 1.000000000000000000 ) ) ;
#5480 = FACE_OUTER_BOUND ( 'NONE', #11849, .T. ) ;
#5481 = ADVANCED_FACE ( 'NONE', ( #868 ), #14585, .T. ) ;
#5482 = EDGE_LOOP ( 'NONE', ( #6474, #8602, #2206, #12134 ) ) ;
#5483 = PRODUCT_DEFINITION_FORMATION_WITH_SPECIFIED_SOURCE ( 'ANY', '', #2051, .NOT_KNOWN. ) ;
#5484 = VECTOR ( 'NONE', #15947, 1000.000000000000000 ) ;
#5485 = LINE ( 'NONE', #11108, #2977 ) ;
#5487 = CIRCLE ( 'NONE', #15942, 12.49999999999999645 ) ;
#5486 = CARTESIAN_POINT ( 'NONE',  ( -71.24615306438090556, 75.97444640456376419, -15.00000000000001421 ) ) ;
#5488 = CARTESIAN_POINT ( 'NONE',  ( -68.99615306438089135, 83.07656473166271383, -167.1454815528550739 ) ) ;
#5489 = ORIENTED_EDGE ( 'NONE', *, *, #15356, .T. ) ;
#5490 = CARTESIAN_POINT ( 'NONE',  ( -68.99615306438093398, 39.70912348813025261, 15.00000000000006928 ) ) ;
#5491 = LINE ( 'NONE', #16805, #2574 ) ;
#5492 = CARTESIAN_POINT ( 'NONE',  ( -75.22571693091748557, 107.3221758769030458, 24.00774849279516232 ) ) ;
#5493 = DIRECTION ( 'NONE',  ( -0.9396926207859103153, 0.3420201433256635504, 0.000000000000000000 ) ) ;
#5494 = FACE_OUTER_BOUND ( 'NONE', #6611, .T. ) ;
#5495 = ORIENTED_EDGE ( 'NONE', *, *, #14997, .F. ) ;
#5496 = EDGE_CURVE ( 'NONE', #18453, #2768, #8318, .T. ) ;
#5497 =( GEOMETRIC_REPRESENTATION_CONTEXT ( 3 ) GLOBAL_UNCERTAINTY_ASSIGNED_CONTEXT ( ( #2550 ) ) GLOBAL_UNIT_ASSIGNED_CONTEXT ( ( #13330, #1723, #9026 ) ) REPRESENTATION_CONTEXT ( 'NONE', 'WORKASPACE' ) );
#5498 = ADVANCED_FACE ( 'NONE', ( #5347 ), #2460, .T. ) ;
#5499 = DIRECTION ( 'NONE',  ( 1.000000000000000000, 0.000000000000000000, 0.000000000000000000 ) ) ;
#5500 = DIRECTION ( 'NONE',  ( 1.000000000000000000, -0.000000000000000000, -0.000000000000000000 ) ) ;
#5501 = SHAPE_REPRESENTATION ( 'hex bolt gradeab fine_iso_ISO 8765 - M8x1.0 x 40 x 22-N', ( #16217 ), #15033 ) ;
#5502 = CARTESIAN_POINT ( 'NONE',  ( -106.3193689061042164, 112.6569076202650450, 102.5000000000000000 ) ) ;
#5503 = CIRCLE ( 'NONE', #5196, 3.999999999999989786 ) ;
#5504 = LINE ( 'NONE', #4106, #11386 ) ;
#5505 = ORIENTED_EDGE ( 'NONE', *, *, #18382, .F. ) ;
#5506 = VECTOR ( 'NONE', #5825, 1000.000000000000000 ) ;
#5507 = ORIENTED_EDGE ( 'NONE', *, *, #3302, .T. ) ;
#5508 = ADVANCED_FACE ( 'NONE', ( #2653 ), #5550, .F. ) ;
#5509 = EDGE_CURVE ( 'NONE', #16233, #14058, #15272, .T. ) ;
#5510 = FACE_OUTER_BOUND ( 'NONE', #11950, .T. ) ;
#5511 = EDGE_CURVE ( 'NONE', #14653, #2315, #6565, .T. ) ;
#5512 = CARTESIAN_POINT ( 'NONE',  ( -3.930119462002491844E-14, -91.08423613455721579, 5.654315315326165603 ) ) ;
#5513 = CARTESIAN_POINT ( 'NONE',  ( -107.5926225674731853, 110.5691553257988460, -26.35917033480641436 ) ) ;
#5514 = EDGE_CURVE ( 'NONE', #12447, #2797, #5448, .T. ) ;
#5515 = CARTESIAN_POINT ( 'NONE',  ( -60.06546592763088910, -91.08423613455721579, -38.97384619189688948 ) ) ;
#5516 = ORIENTED_EDGE ( 'NONE', *, *, #9247, .F. ) ;
#5517 = CIRCLE ( 'NONE', #1352, 5.000000000000004441 ) ;
#5518 = CARTESIAN_POINT ( 'NONE',  ( -66.32832664217301044, 109.6035164793382393, -28.00000000000000355 ) ) ;
#5519 = AXIS2_PLACEMENT_3D ( 'NONE', #11491, #10346, #240 ) ;
#5520 = CARTESIAN_POINT ( 'NONE',  ( 0.000000000000000000, 5.629165124598801917, 3.250000000000037748 ) ) ;
#5521 = CARTESIAN_POINT ( 'NONE',  ( -57.08002265617300708, 84.22855780814606419, 37.50000000000000000 ) ) ;
#5522 = CIRCLE ( 'NONE', #1932, 26.04359719766049608 ) ;
#5523 = LINE ( 'NONE', #18151, #2151 ) ;
#5524 = PRODUCT ( 'MAS-321', 'MAS-321', '', ( #3779 ) ) ;
#5525 = VERTEX_POINT ( 'NONE', #2354 ) ;
#5526 = EDGE_CURVE ( 'NONE', #6870, #13041, #8270, .T. ) ;
#5527 = CARTESIAN_POINT ( 'NONE',  ( -71.24615306438070661, 137.9174286652292096, -167.1454815528550739 ) ) ;
#5528 = ORIENTED_EDGE ( 'NONE', *, *, #13180, .F. ) ;
#5529 = AXIS2_PLACEMENT_3D ( 'NONE', #4602, #10129, #14694 ) ;
#5530 = CARTESIAN_POINT ( 'NONE',  ( -25.66933353722515676, -96.08423613455721579, -5.654315315325675328 ) ) ;
#5531 = LINE ( 'NONE', #10192, #12526 ) ;
#5532 = EDGE_LOOP ( 'NONE', ( #4807, #17906, #17522, #13251 ) ) ;
#5533 = ORIENTED_EDGE ( 'NONE', *, *, #7750, .F. ) ;
#5534 = AXIS2_PLACEMENT_3D ( 'NONE', #9352, #16722, #10951 ) ;
#5535 = ORIENTED_EDGE ( 'NONE', *, *, #11354, .T. ) ;
#5536 = CARTESIAN_POINT ( 'NONE',  ( -68.99615306438077766, 124.5321250381302747, -15.00000000000001421 ) ) ;
#5537 = FACE_OUTER_BOUND ( 'NONE', #16204, .T. ) ;
#5538 = CARTESIAN_POINT ( 'NONE',  ( -71.24615306438117557, 5.970537365229261262, 15.00000000000006928 ) ) ;
#5539 = DIRECTION ( 'NONE',  ( 0.000000000000000000, 0.000000000000000000, 1.000000000000000000 ) ) ;
#5540 = CARTESIAN_POINT ( 'NONE',  ( -207.6107609645051753, 84.22855780814606419, 62.50000000000001421 ) ) ;
#5541 = ORIENTED_EDGE ( 'NONE', *, *, #17734, .T. ) ;
#5542 = AXIS2_PLACEMENT_3D ( 'NONE', #3367, #9091, #3644 ) ;
#5543 = DIRECTION ( 'NONE',  ( -0.9396926207859171987, 0.3420201433256444545, 1.086737899652999999E-16 ) ) ;
#5544 = ORIENTED_EDGE ( 'NONE', *, *, #17275, .T. ) ;
#5545 = CARTESIAN_POINT ( 'NONE',  ( -68.99615306438117557, 1.395155831662692192, 15.00000000000006928 ) ) ;
#5546 = AXIS2_PLACEMENT_3D ( 'NONE', #15523, #8424, #15884 ) ;
#5547 = CIRCLE ( 'NONE', #12113, 6.500000000000039968 ) ;
#5548 = CARTESIAN_POINT ( 'NONE',  ( -71.24615306438110451, 19.42577870456376843, -15.00000000000001421 ) ) ;
#5549 = ORIENTED_EDGE ( 'NONE', *, *, #7890, .F. ) ;
#5550 = PLANE ( 'NONE',  #11006 ) ;
#5551 = ORIENTED_EDGE ( 'NONE', *, *, #18201, .F. ) ;
#5552 = ORIENTED_EDGE ( 'NONE', *, *, #11559, .F. ) ;
#5553 =( NAMED_UNIT ( * ) PLANE_ANGLE_UNIT ( ) SI_UNIT ( $, .RADIAN. ) );
#5554 = CARTESIAN_POINT ( 'NONE',  ( -107.5926225674731711, 57.88796029049330372, 22.33417033480641223 ) ) ;
#5555 = CARTESIAN_POINT ( 'NONE',  ( -92.59262256747321373, 110.5691553257988460, 26.35917033480641436 ) ) ;
#5556 = ORIENTED_EDGE ( 'NONE', *, *, #6058, .T. ) ;
#5557 = ORIENTED_EDGE ( 'NONE', *, *, #12007, .T. ) ;
#5558 = CARTESIAN_POINT ( 'NONE',  ( -23.71312654895687189, 50.37139919635580299, -27.05770456752418696 ) ) ;
#5559 = CARTESIAN_POINT ( 'NONE',  ( -49.58002265617300708, 84.22855780814606419, -167.1454815528550739 ) ) ;
#5560 = VERTEX_POINT ( 'NONE', #12395 ) ;
#5561 = CARTESIAN_POINT ( 'NONE',  ( -54.78701292294434211, 94.21775734381050427, -167.1454815528550739 ) ) ;
#5562 = CARTESIAN_POINT ( 'NONE',  ( -70.06856178257680767, 110.5691553257988460, 22.35917033480641791 ) ) ;
#5563 = FACE_OUTER_BOUND ( 'NONE', #10523, .T. ) ;
#5564 = VERTEX_POINT ( 'NONE', #15378 ) ;
#5565 = CARTESIAN_POINT ( 'NONE',  ( -70.47187574892673467, 110.3702813545971679, -22.35917033480642147 ) ) ;
#5566 = CARTESIAN_POINT ( 'NONE',  ( -68.99615306438080609, 108.2093059316626693, -167.1454815528550739 ) ) ;
#5567 = VERTEX_POINT ( 'NONE', #2569 ) ;
#5568 = DIRECTION ( 'NONE',  ( 0.9396926207859078728, 0.3420201433256701007, 0.000000000000000000 ) ) ;
#5569 = ORIENTED_EDGE ( 'NONE', *, *, #13838, .F. ) ;
#5570 = ADVANCED_FACE ( 'NONE', ( #14064 ), #12292, .T. ) ;
#5571 = DIRECTION ( 'NONE',  ( -0.9475106458593564041, -0.3197242186372270534, 0.000000000000000000 ) ) ;
#5572 = VERTEX_POINT ( 'NONE', #13979 ) ;
#5573 = CARTESIAN_POINT ( 'NONE',  ( -67.59262256747317110, 56.80567558672318995, 22.50837044127973030 ) ) ;
#5574 = CARTESIAN_POINT ( 'NONE',  ( -68.99615306438111872, 14.57638228813026871, -167.1454815528550739 ) ) ;
#5575 = ORIENTED_EDGE ( 'NONE', *, *, #7982, .T. ) ;
#5576 = EDGE_CURVE ( 'NONE', #10635, #16643, #6671, .T. ) ;
#5577 = DIRECTION ( 'NONE',  ( 0.000000000000000000, 0.000000000000000000, 1.000000000000000000 ) ) ;
#5578 = DIRECTION ( 'NONE',  ( 1.156482317317869999E-16, 0.000000000000000000, 1.000000000000000000 ) ) ;
#5579 = DIRECTION ( 'NONE',  ( -1.000000000000000000, 0.000000000000000000, 0.000000000000000000 ) ) ;
#5580 = CARTESIAN_POINT ( 'NONE',  ( -68.99615306438067819, 146.5232735881302801, 15.00000000000006928 ) ) ;
#5581 = EDGE_LOOP ( 'NONE', ( #7254, #18182, #14154, #16294 ) ) ;
#5582 = CARTESIAN_POINT ( 'NONE',  ( -67.20241558018224737, 85.83453492254335515, 15.00000000000006928 ) ) ;
#5583 = DIRECTION ( 'NONE',  ( 0.000000000000000000, 0.000000000000000000, 1.000000000000000000 ) ) ;
#5584 = DIRECTION ( 'NONE',  ( 1.000000000000000000, 0.000000000000000000, 3.771137991253928573E-16 ) ) ;
#5585 = CARTESIAN_POINT ( 'NONE',  ( 5.299999999999998934, 4.351979364426058414E-16, -6.499999999999999112 ) ) ;
#5586 = EDGE_LOOP ( 'NONE', ( #15005, #1794, #12689, #17874 ) ) ;
#5587 = CARTESIAN_POINT ( 'NONE',  ( -25.66933353722515676, -91.08423613455721579, 5.654315315325685987 ) ) ;
#5588 = LINE ( 'NONE', #14021, #3520 ) ;
#5589 = EDGE_CURVE ( 'NONE', #3055, #3490, #16959, .T. ) ;
#5590 = DIRECTION ( 'NONE',  ( 1.000000000000000000, 0.000000000000000000, 0.000000000000000000 ) ) ;
#5591 = DIRECTION ( 'NONE',  ( -1.000000000000000000, 0.000000000000000000, 0.000000000000000000 ) ) ;
#5592 = ORIENTED_EDGE ( 'NONE', *, *, #12204, .T. ) ;
#5593 = ORIENTED_EDGE ( 'NONE', *, *, #13977, .T. ) ;
#5594 = FACE_OUTER_BOUND ( 'NONE', #9691, .T. ) ;
#5595 = ADVANCED_FACE ( 'NONE', ( #18092 ), #18275, .T. ) ;
#5596 = ORIENTED_EDGE ( 'NONE', *, *, #1958, .T. ) ;
#5597 = ADVANCED_FACE ( 'NONE', ( #8061 ), #13692, .T. ) ;
#5598 = DIRECTION ( 'NONE',  ( 0.000000000000000000, 0.000000000000000000, 1.000000000000000000 ) ) ;
#5599 = LINE ( 'NONE', #8127, #12041 ) ;
#5600 = DIRECTION ( 'NONE',  ( 0.000000000000000000, 1.000000000000000000, 0.000000000000000000 ) ) ;
#5601 = ORIENTED_EDGE ( 'NONE', *, *, #11577, .F. ) ;
#5602 = CARTESIAN_POINT ( 'NONE',  ( 15.23320273812466041, -19.34983604512934363, 3.000000000000000000 ) ) ;
#5603 = CYLINDRICAL_SURFACE ( 'NONE', #15420, 4.599999999999999645 ) ;
#5604 = FACE_OUTER_BOUND ( 'NONE', #14244, .T. ) ;
#5605 = LINE ( 'NONE', #12823, #5445 ) ;
#5606 = ORIENTED_EDGE ( 'NONE', *, *, #5925, .F. ) ;
#5607 = ADVANCED_FACE ( 'NONE', ( #5266 ), #14341, .F. ) ;
#5608 = B_SPLINE_CURVE_WITH_KNOTS ( 'NONE', 3,
 ( #18513, #3914, #1211, #11031, #2808, #11133, #14125, #17007 ),
 .UNSPECIFIED., .F., .F.,
 ( 4, 2, 2, 4 ),
 ( 0.003797433802554432431, 0.004743183970586246564, 0.005688934138618060264, 0.007580434474681690266 ),
 .UNSPECIFIED. ) ;
#5609 = DIRECTION ( 'NONE',  ( 0.000000000000000000, 0.000000000000000000, 1.000000000000000000 ) ) ;
#5610 = EDGE_CURVE ( 'NONE', #17762, #5426, #7412, .T. ) ;
#5611 = ORIENTED_EDGE ( 'NONE', *, *, #12373, .T. ) ;
#5612 = EDGE_CURVE ( 'NONE', #16752, #9640, #14162, .T. ) ;
#5613 = FACE_OUTER_BOUND ( 'NONE', #4739, .T. ) ;
#5614 = CARTESIAN_POINT ( 'NONE',  ( -71.24615306438117557, 5.970537365229261262, 15.00000000000006928 ) ) ;
#5615 = ORIENTED_EDGE ( 'NONE', *, *, #11685, .T. ) ;
#5616 =( REPRESENTATION_RELATIONSHIP ('NONE','NONE', #359, #8623 ) REPRESENTATION_RELATIONSHIP_WITH_TRANSFORMATION ( #8178 )SHAPE_REPRESENTATION_RELATIONSHIP( ) );
#5617 = EDGE_CURVE ( 'NONE', #9665, #6928, #10314, .T. ) ;
#5618 = ORIENTED_EDGE ( 'NONE', *, *, #4456, .T. ) ;
#5619 = ORIENTED_EDGE ( 'NONE', *, *, #3079, .F. ) ;
#5620 = EDGE_CURVE ( 'NONE', #7505, #9854, #1739, .T. ) ;
#5621 = EDGE_CURVE ( 'NONE', #5840, #1115, #6001, .T. ) ;
#5622 = ADVANCED_FACE ( 'NONE', ( #5900 ), #4332, .T. ) ;
#5623 = DIRECTION ( 'NONE',  ( 0.9396926207859084279, 0.3420201433256686574, 0.000000000000000000 ) ) ;
#5624 = DIRECTION ( 'NONE',  ( -1.000000000000000000, 0.000000000000000000, 1.387778780781445182E-16 ) ) ;
#5625 = CARTESIAN_POINT ( 'NONE',  ( -71.24615306438076345, 126.2399288045637462, -15.00000000000001421 ) ) ;
#5626 = EDGE_CURVE ( 'NONE', #2271, #15616, #14297, .T. ) ;
#5627 = CARTESIAN_POINT ( 'NONE',  ( -56.59294758719027385, 94.46597735006069740, -167.1454815528550739 ) ) ;
#5628 = DIRECTION ( 'NONE',  ( 0.000000000000000000, 0.000000000000000000, -1.000000000000000000 ) ) ;
#5629 = ORIENTED_EDGE ( 'NONE', *, *, #12634, .F. ) ;
#5630 = CYLINDRICAL_SURFACE ( 'NONE', #11413, 4.599999999999992539 ) ;
#5631 = ORIENTED_EDGE ( 'NONE', *, *, #9951, .F. ) ;
#5632 = CARTESIAN_POINT ( 'NONE',  ( -71.24615306438086293, 94.82400230456377699, -167.1454815528550739 ) ) ;
#5633 = CARTESIAN_POINT ( 'NONE',  ( 9.543663295069050534, 56.41207303426870112, 7.000000000000010658 ) ) ;
#5634 = AXIS2_PLACEMENT_3D ( 'NONE', #8732, #290, #17404 ) ;
#5635 = ORIENTED_EDGE ( 'NONE', *, *, #9586, .T. ) ;
#5636 = CARTESIAN_POINT ( 'NONE',  ( -114.6525958062275095, -93.09900722835551790, -6.628862765693821046 ) ) ;
#5637 = ADVANCED_FACE ( 'NONE', ( #8637 ), #6191, .T. ) ;
#5638 = ORIENTED_EDGE ( 'NONE', *, *, #12667, .T. ) ;
#5639 = ADVANCED_FACE ( 'NONE', ( #14259 ), #17312, .T. ) ;
#5640 = ORIENTED_EDGE ( 'NONE', *, *, #14773, .T. ) ;
#5641 = SURFACE_STYLE_FILL_AREA ( #18280 ) ;
#5642 = AXIS2_PLACEMENT_3D ( 'NONE', #11887, #4760, #16281 ) ;
#5643 = DIRECTION ( 'NONE',  ( 4.675871521838984962E-16, -1.000000000000000000, 0.000000000000000000 ) ) ;
#5644 = LINE ( 'NONE', #8276, #6956 ) ;
#5645 = ORIENTED_EDGE ( 'NONE', *, *, #1041, .T. ) ;
#5646 = ORIENTED_EDGE ( 'NONE', *, *, #12858, .F. ) ;
#5647 = DIRECTION ( 'NONE',  ( 1.000000000000000000, -0.000000000000000000, -0.000000000000000000 ) ) ;
#5648 = CARTESIAN_POINT ( 'NONE',  ( -68.99615306438111872, 20.24471173166267590, -15.00000000000001421 ) ) ;
#5649 = VERTEX_POINT ( 'NONE', #17230 ) ;
#5650 = CARTESIAN_POINT ( 'NONE',  ( -68.99615306438077766, 117.6340838816626899, -167.1454815528550739 ) ) ;
#5651 = CARTESIAN_POINT ( 'NONE',  ( -70.71978124295708312, -111.0842361345572158, 28.18308811886538479 ) ) ;
#5652 = LINE ( 'NONE', #4163, #17989 ) ;
#5653 = ORIENTED_EDGE ( 'NONE', *, *, #16946, .F. ) ;
#5654 = DIRECTION ( 'NONE',  ( -1.000000000000000000, 0.000000000000000000, 0.000000000000000000 ) ) ;
#5655 = ORIENTED_EDGE ( 'NONE', *, *, #13286, .F. ) ;
#5656 = ORIENTED_EDGE ( 'NONE', *, *, #5402, .T. ) ;
#5657 = AXIS2_PLACEMENT_3D ( 'NONE', #6799, #13918, #15496 ) ;
#5658 = CARTESIAN_POINT ( 'NONE',  ( -92.59262256747319952, 60.58224449241411946, -25.00000000000000000 ) ) ;
#5659 = VECTOR ( 'NONE', #994, 1000.000000000000000 ) ;
#5660 = VERTEX_POINT ( 'NONE', #12954 ) ;
#5661 = ORIENTED_EDGE ( 'NONE', *, *, #3673, .T. ) ;
#5662 = CARTESIAN_POINT ( 'NONE',  ( -68.99615306438070661, 137.0984956381303164, 15.00000000000006928 ) ) ;
#5663 = ORIENTED_EDGE ( 'NONE', *, *, #9799, .T. ) ;
#5664 = CARTESIAN_POINT ( 'NONE',  ( -68.99615306438091977, 73.65178678166269322, -167.1454815528550739 ) ) ;
#5665 = FACE_OUTER_BOUND ( 'NONE', #9450, .T. ) ;
#5666 = DIRECTION ( 'NONE',  ( 0.000000000000000000, 0.000000000000000000, 1.000000000000000000 ) ) ;
#5667 = AXIS2_PLACEMENT_3D ( 'NONE', #17073, #14355, #15583 ) ;
#5668 = CARTESIAN_POINT ( 'NONE',  ( -71.24615306438097662, 56.23601976522923707, -167.1454815528550739 ) ) ;
#5669 = ORIENTED_EDGE ( 'NONE', *, *, #16915, .F. ) ;
#5670 = ADVANCED_FACE ( 'NONE', ( #5818 ), #16982, .T. ) ;
#5671 = DIRECTION ( 'NONE',  ( 0.000000000000000000, 1.000000000000000000, 0.000000000000000000 ) ) ;
#5672 = CARTESIAN_POINT ( 'NONE',  ( -68.99615306438082030, 102.5409764881302692, -15.00000000000001421 ) ) ;
#5673 = DIRECTION ( 'NONE',  ( -0.9396926207859168656, 0.3420201433256456203, 0.000000000000000000 ) ) ;
#5674 = VERTEX_POINT ( 'NONE', #4414 ) ;
#5675 = EDGE_CURVE ( 'NONE', #3839, #2191, #17875, .T. ) ;
#5676 = DIRECTION ( 'NONE',  ( 0.3420201433256724322, 0.9396926207859070956, -0.000000000000000000 ) ) ;
#5677 = CARTESIAN_POINT ( 'NONE',  ( -107.5926225674731711, 57.88796029049330372, -30.38417033480641294 ) ) ;
#5678 = CARTESIAN_POINT ( 'NONE',  ( -68.99615306438111872, 11.43478963813029914, -167.1454815528550739 ) ) ;
#5679 = CARTESIAN_POINT ( 'NONE',  ( -68.99615306438083451, 98.78452798166264870, 15.00000000000006928 ) ) ;
#5680 = ORIENTED_EDGE ( 'NONE', *, *, #8605, .F. ) ;
#5681 = AXIS2_PLACEMENT_3D ( 'NONE', #2843, #7138, #12949 ) ;
#5682 = ORIENTED_EDGE ( 'NONE', *, *, #16936, .T. ) ;
#5683 = VECTOR ( 'NONE', #17665, 1000.000000000000000 ) ;
#5684 = DIRECTION ( 'NONE',  ( 0.9396926207859171987, 0.3420201433256444545, 0.000000000000000000 ) ) ;
#5685 = VERTEX_POINT ( 'NONE', #662 ) ;
#5686 = CARTESIAN_POINT ( 'NONE',  ( -67.59262256747317110, 57.88796029049329661, 30.35917033480639660 ) ) ;
#5687 = DIRECTION ( 'NONE',  ( 1.000000000000000000, 0.000000000000000000, 0.000000000000000000 ) ) ;
#5688 = EDGE_LOOP ( 'NONE', ( #1847, #1765, #12868, #11563, #10625, #11328 ) ) ;
#5689 = AXIS2_PLACEMENT_3D ( 'NONE', #16260, #8887, #4944 ) ;
#5690 = CARTESIAN_POINT ( 'NONE',  ( -66.75310480962880888, 108.5438542518999725, -28.00000000000000711 ) ) ;
#5691 = DIRECTION ( 'NONE',  ( 1.000000000000000000, 0.000000000000000000, 5.551115123125780730E-16 ) ) ;
#5692 = DIRECTION ( 'NONE',  ( 0.000000000000000000, 0.000000000000000000, 1.000000000000000000 ) ) ;
#5693 = DIRECTION ( 'NONE',  ( 0.000000000000000000, 0.000000000000000000, 1.000000000000000000 ) ) ;
#5694 = ORIENTED_EDGE ( 'NONE', *, *, #13618, .F. ) ;
#5695 = CIRCLE ( 'NONE', #4487, 7.168074330098680669 ) ;
#5696 = VECTOR ( 'NONE', #7827, 1000.000000000000000 ) ;
#5697 = DIRECTION ( 'NONE',  ( -0.000000000000000000, 1.000000000000000000, -0.000000000000000000 ) ) ;
#5698 = EDGE_LOOP ( 'NONE', ( #14722, #5645, #3928, #16433 ) ) ;
#5699 = EDGE_CURVE ( 'NONE', #13839, #9806, #12084, .T. ) ;
#5700 = DIRECTION ( 'NONE',  ( 0.000000000000000000, 0.000000000000000000, 1.000000000000000000 ) ) ;
#5701 = LINE ( 'NONE', #4311, #6203 ) ;
#5702 = ORIENTED_EDGE ( 'NONE', *, *, #7739, .T. ) ;
#5703 = VERTEX_POINT ( 'NONE', #2152 ) ;
#5704 = AXIS2_PLACEMENT_3D ( 'NONE', #16295, #17793, #17692 ) ;
#5705 = ORIENTED_EDGE ( 'NONE', *, *, #13085, .T. ) ;
#5706 = VECTOR ( 'NONE', #9213, 1000.000000000000000 ) ;
#5707 = CONICAL_SURFACE ( 'NONE', #45, 3.999999999999989786, 1.029744258676652091 ) ;
#5708 = CARTESIAN_POINT ( 'NONE',  ( 95.45835937779683888, -32.62665103886254059, 7.000000000000010658 ) ) ;
#5709 = LINE ( 'NONE', #9650, #385 ) ;
#5710 = ADVANCED_FACE ( 'NONE', ( #16010 ), #14016, .T. ) ;
#5711 = DIRECTION ( 'NONE',  ( -0.9396926207859097602, 0.3420201433256649937, 0.000000000000000000 ) ) ;
#5712 = EDGE_CURVE ( 'NONE', #9457, #1289, #9832, .T. ) ;
#5713 = CARTESIAN_POINT ( 'NONE',  ( -68.99615306438106188, 27.14275288813031040, -167.1454815528550739 ) ) ;
#5714 = DIRECTION ( 'NONE',  ( -0.000000000000000000, -0.000000000000000000, 1.000000000000000000 ) ) ;
#5715 = ORIENTED_EDGE ( 'NONE', *, *, #3675, .T. ) ;
#5716 = CARTESIAN_POINT ( 'NONE',  ( -92.59262256747319952, 54.12595869546677818, -25.00000000000000000 ) ) ;
#5717 = VERTEX_POINT ( 'NONE', #11978 ) ;
#5718 = AXIS2_PLACEMENT_3D ( 'NONE', #17974, #5160, #16569 ) ;
#5719 = CARTESIAN_POINT ( 'NONE',  ( -78.76908973550909820, -91.80660034481553566, 42.25011218277849423 ) ) ;
#5720 = DIRECTION ( 'NONE',  ( 0.000000000000000000, 1.224646799147353207E-16, 1.000000000000000000 ) ) ;
#5721 = VERTEX_POINT ( 'NONE', #17578 ) ;
#5722 = EDGE_CURVE ( 'NONE', #6290, #715, #4153, .T. ) ;
#5723 = EDGE_CURVE ( 'NONE', #4262, #3659, #7715, .T. ) ;
#5724 = VECTOR ( 'NONE', #860, 1000.000000000000000 ) ;
#5725 = EDGE_CURVE ( 'NONE', #2362, #12457, #3470, .T. ) ;
#5726 = AXIS2_PLACEMENT_3D ( 'NONE', #7951, #840, #2143 ) ;
#5727 = CARTESIAN_POINT ( 'NONE',  ( -109.6936274348538944, -91.08423613455721579, -10.65431531532595777 ) ) ;
#5728 = ORIENTED_EDGE ( 'NONE', *, *, #15103, .F. ) ;
#5729 = ORIENTED_EDGE ( 'NONE', *, *, #13159, .F. ) ;
#5730 = EDGE_CURVE ( 'NONE', #15130, #9307, #17575, .T. ) ;
#5731 = VECTOR ( 'NONE', #16499, 1000.000000000000114 ) ;
#5732 = CARTESIAN_POINT ( 'NONE',  ( -71.24615306438103346, 43.66964916522919538, 15.00000000000006928 ) ) ;
#5733 = CARTESIAN_POINT ( 'NONE',  ( -71.24615306438084872, 88.54081700456373483, -15.00000000000001421 ) ) ;
#5734 = CARTESIAN_POINT ( 'NONE',  ( -71.24615306438076345, 131.6342433652292243, -15.00000000000001421 ) ) ;
#5735 = VERTEX_POINT ( 'NONE', #17676 ) ;
#5736 = AXIS2_PLACEMENT_3D ( 'NONE', #11121, #16808, #4001 ) ;
#5737 = ORIENTED_EDGE ( 'NONE', *, *, #3319, .F. ) ;
#5738 = AXIS2_PLACEMENT_3D ( 'NONE', #11860, #4832, #2369 ) ;
#5739 = EDGE_CURVE ( 'NONE', #12968, #12199, #4961, .T. ) ;
#5740 = ADVANCED_FACE ( 'NONE', ( #16179 ), #10123, .F. ) ;
#5741 = CARTESIAN_POINT ( 'NONE',  ( -68.99615306438089135, 83.69142058813029905, -15.00000000000001421 ) ) ;
#5742 = VERTEX_POINT ( 'NONE', #16363 ) ;
#5743 = FACE_OUTER_BOUND ( 'NONE', #9076, .T. ) ;
#5744 = CARTESIAN_POINT ( 'NONE',  ( -71.24615306438070661, 141.0590213152292449, -15.00000000000001421 ) ) ;
#5745 = CARTESIAN_POINT ( 'NONE',  ( -97.59262256747321373, 110.5691553257988460, -22.35917033480641791 ) ) ;
#5746 = ORIENTED_EDGE ( 'NONE', *, *, #10396, .F. ) ;
#5747 = DIRECTION ( 'NONE',  ( -1.000000000000000000, -7.442644330182800165E-16, 0.000000000000000000 ) ) ;
#5748 = ORIENTED_EDGE ( 'NONE', *, *, #17130, .F. ) ;
#5749 = ADVANCED_FACE ( 'NONE', ( #1980 ), #4864, .T. ) ;
#5750 = CIRCLE ( 'NONE', #6638, 7.500000000000007105 ) ;
#5751 = ORIENTED_EDGE ( 'NONE', *, *, #6626, .F. ) ;
#5752 = FACE_OUTER_BOUND ( 'NONE', #17274, .T. ) ;
#5753 = CIRCLE ( 'NONE', #15915, 6.500000000000039968 ) ;
#5754 = VERTEX_POINT ( 'NONE', #6163 ) ;
#5755 = DIRECTION ( 'NONE',  ( 1.000000000000000000, 0.000000000000000000, 0.000000000000000000 ) ) ;
#5756 = CARTESIAN_POINT ( 'NONE',  ( -47.76628296033400289, 88.50596986196467242, -15.00000000000001421 ) ) ;
#5757 = CIRCLE ( 'NONE', #9648, 10.65431531532568243 ) ;
#5758 = ORIENTED_EDGE ( 'NONE', *, *, #6284, .T. ) ;
#5759 = LINE ( 'NONE', #163, #4184 ) ;
#5760 = DIRECTION ( 'NONE',  ( 0.000000000000000000, 1.000000000000000000, 0.000000000000000000 ) ) ;
#5761 = DIRECTION ( 'NONE',  ( 0.000000000000000000, 1.000000000000000000, 0.000000000000000000 ) ) ;
#5762 = CYLINDRICAL_SURFACE ( 'NONE', #5519, 22.04359719766050318 ) ;
#5763 = EDGE_LOOP ( 'NONE', ( #18429, #14805, #17005, #3614 ) ) ;
#5764 = DIRECTION ( 'NONE',  ( 0.000000000000000000, 0.000000000000000000, -1.000000000000000000 ) ) ;
#5765 = VECTOR ( 'NONE', #11608, 1000.000000000000000 ) ;
#5766 = CONICAL_SURFACE ( 'NONE', #8157, 4.025000000000000355, 0.7853981633975870569 ) ;
#5767 = VECTOR ( 'NONE', #5259, 1000.000000000000000 ) ;
#5768 = PLANE ( 'NONE',  #15617 ) ;
#5769 = CARTESIAN_POINT ( 'NONE',  ( -64.09025127992789805, 84.22855780814606419, 28.00000000000000355 ) ) ;
#5770 = ORIENTED_EDGE ( 'NONE', *, *, #1041, .F. ) ;
#5771 = CARTESIAN_POINT ( 'NONE',  ( -107.5926225674731995, 60.58224449241411946, 35.00000000000000000 ) ) ;
#5772 = VECTOR ( 'NONE', #6996, 1000.000000000000114 ) ;
#5773 = DIRECTION ( 'NONE',  ( 1.000000000000000000, 0.000000000000000000, 0.000000000000000000 ) ) ;
#5774 = DIRECTION ( 'NONE',  ( 0.000000000000000000, 1.000000000000000000, 0.000000000000000000 ) ) ;
#5775 = ORIENTED_EDGE ( 'NONE', *, *, #7680, .F. ) ;
#5776 = VERTEX_POINT ( 'NONE', #17499 ) ;
#5777 = VECTOR ( 'NONE', #4526, 1000.000000000000000 ) ;
#5778 = CARTESIAN_POINT ( 'NONE',  ( -68.99615306438111872, 20.24471173166267235, -167.1454815528550739 ) ) ;
#5779 = VERTEX_POINT ( 'NONE', #14601 ) ;
#5780 = CARTESIAN_POINT ( 'NONE',  ( -67.02098183716937285, 79.99098546104525553, -167.1454815528550739 ) ) ;
#5781 = CARTESIAN_POINT ( 'NONE',  ( 0.000000000000000000, 0.000000000000000000, 0.000000000000000000 ) ) ;
#5782 = DIRECTION ( 'NONE',  ( 1.000000000000000000, 0.000000000000000000, 0.000000000000000000 ) ) ;
#5783 = CARTESIAN_POINT ( 'NONE',  ( -60.58685171690446225, -91.10977296152348970, -39.65137083761668890 ) ) ;
#5784 = VERTEX_POINT ( 'NONE', #7494 ) ;
#5785 = CARTESIAN_POINT ( 'NONE',  ( 45.30000000000000426, 2.492512489064173907E-16, -3.445500000000000451 ) ) ;
#5786 = CARTESIAN_POINT ( 'NONE',  ( -68.12361985383350316, 84.22855780814606419, 37.50000000000000000 ) ) ;
#5787 = LINE ( 'NONE', #13015, #17675 ) ;
#5788 = ORIENTED_EDGE ( 'NONE', *, *, #10166, .F. ) ;
#5789 = DIRECTION ( 'NONE',  ( -5.204170427930409450E-16, 0.000000000000000000, 1.000000000000000000 ) ) ;
#5790 = CIRCLE ( 'NONE', #14183, 4.600000000000013856 ) ;
#5791 = VECTOR ( 'NONE', #3863, 999.9999999999998863 ) ;
#5792 = DIRECTION ( 'NONE',  ( 0.9396926207859097602, 0.3420201433256649937, 0.000000000000000000 ) ) ;
#5793 = ORIENTED_EDGE ( 'NONE', *, *, #15805, .F. ) ;
#5794 = DIRECTION ( 'NONE',  ( 1.000000000000000000, 0.000000000000000000, 0.000000000000000000 ) ) ;
#5795 = DIRECTION ( 'NONE',  ( 0.000000000000000000, 1.000000000000000000, 0.000000000000000000 ) ) ;
#5796 = ORIENTED_EDGE ( 'NONE', *, *, #8767, .F. ) ;
#5797 = EDGE_LOOP ( 'NONE', ( #15037, #1414, #11077, #13591 ) ) ;
#5798 = VECTOR ( 'NONE', #13109, 1000.000000000000000 ) ;
#5799 = AXIS2_PLACEMENT_3D ( 'NONE', #16995, #14613, #1712 ) ;
#5800 = CIRCLE ( 'NONE', #7899, 10.38004356723770627 ) ;
#5801 = B_SPLINE_CURVE_WITH_KNOTS ( 'NONE', 3,
 ( #11880, #4754, #9086, #1974, #11307, #1390, #16807, #8504, #16997, #8303, #8211, #14017, #14113, #12335, #15606, #7004, #11219, #4100, #9712, #18028, #13823, #18420, #12527, #9804, #14211, #2504, #13928, #1113 ),
 .UNSPECIFIED., .F., .F.,
 ( 4, 2, 2, 2, 2, 2, 2, 2, 2, 2, 2, 2, 2, 4 ),
 ( 0.000000000000000000, 0.01246990002149389425, 0.01870485003224084050, 0.02182232503761430756, 0.02493980004298777114, 0.03740970006448163937, 0.04364465007522858736, 0.04676212508060205442, 0.04987960008597552147, 0.06234950010746938276, 0.07481940012896323711, 0.08105435013971017122, 0.08728930015045711921, 0.09975920017195097356 ),
 .UNSPECIFIED. ) ;
#5802 = VECTOR ( 'NONE', #8833, 1000.000000000000000 ) ;
#5803 = CARTESIAN_POINT ( 'NONE',  ( -70.71978124295696944, -141.5628872026273086, 18.23991632971911514 ) ) ;
#5804 = DIRECTION ( 'NONE',  ( -0.000000000000000000, -0.000000000000000000, -1.000000000000000000 ) ) ;
#5805 = CARTESIAN_POINT ( 'NONE',  ( -78.03414724812056136, 82.27553650601716129, 69.74547876954885339 ) ) ;
#5806 = EDGE_CURVE ( 'NONE', #12040, #12836, #13479, .T. ) ;
#5807 = LINE ( 'NONE', #15458, #15532 ) ;
#5808 = CYLINDRICAL_SURFACE ( 'NONE', #4236, 10.24899999999998812 ) ;
#5809 = ORIENTED_EDGE ( 'NONE', *, *, #13067, .T. ) ;
#5810 = VECTOR ( 'NONE', #13691, 1000.000000000000000 ) ;
#5811 = CARTESIAN_POINT ( 'NONE',  ( 5.299999999999998934, 7.505553499465141165, -1.387778780781445676E-14 ) ) ;
#5812 = ORIENTED_EDGE ( 'NONE', *, *, #10984, .T. ) ;
#5813 = DIRECTION ( 'NONE',  ( 1.156482317317869999E-16, 0.000000000000000000, 1.000000000000000000 ) ) ;
#5814 = FACE_OUTER_BOUND ( 'NONE', #6725, .T. ) ;
#5815 = ORIENTED_EDGE ( 'NONE', *, *, #10396, .T. ) ;
#5816 = AXIS2_PLACEMENT_3D ( 'NONE', #14823, #6490, #13427 ) ;
#5817 = AXIS2_PLACEMENT_3D ( 'NONE', #7484, #475, #2940 ) ;
#5818 = FACE_OUTER_BOUND ( 'NONE', #11934, .T. ) ;
#5820 = EDGE_LOOP ( 'NONE', ( #10610, #14671, #3455, #345 ) ) ;
#5819 = AXIS2_PLACEMENT_3D ( 'NONE', #12066, #7946, #10465 ) ;
#5821 = EDGE_CURVE ( 'NONE', #16605, #8708, #13307, .T. ) ;
#5822 = EDGE_CURVE ( 'NONE', #5735, #4782, #10393, .T. ) ;
#5823 = ORIENTED_EDGE ( 'NONE', *, *, #6637, .T. ) ;
#5824 = CARTESIAN_POINT ( 'NONE',  ( -68.99615306438066398, 146.5232735881302801, -15.00000000000001421 ) ) ;
#5825 = DIRECTION ( 'NONE',  ( 0.000000000000000000, 1.000000000000000000, 0.000000000000000000 ) ) ;
#5826 = CARTESIAN_POINT ( 'NONE',  ( 0.000000000000000000, 5.629165124598801917, 3.250000000000037748 ) ) ;
#5827 = AXIS2_PLACEMENT_3D ( 'NONE', #11713, #11886, #14600 ) ;
#5828 = EDGE_CURVE ( 'NONE', #7123, #1024, #6453, .T. ) ;
#5829 = ORIENTED_EDGE ( 'NONE', *, *, #9043, .T. ) ;
#5830 = EDGE_CURVE ( 'NONE', #4, #17405, #7765, .T. ) ;
#5831 = CIRCLE ( 'NONE', #5845, 4.599999999999992539 ) ;
#5832 = AXIS2_PLACEMENT_3D ( 'NONE', #4823, #16239, #17542 ) ;
#5833 = ORIENTED_EDGE ( 'NONE', *, *, #1074, .F. ) ;
#5834 = LINE ( 'NONE', #14450, #4220 ) ;
#5835 = EDGE_CURVE ( 'NONE', #1745, #5859, #4680, .T. ) ;
#5836 = CARTESIAN_POINT ( 'NONE',  ( -56.16856596726385220, 74.02016676429185793, -15.00000000000001421 ) ) ;
#5837 = DIRECTION ( 'NONE',  ( -1.000000000000000000, 0.000000000000000000, 0.000000000000000000 ) ) ;
#5838 = ORIENTED_EDGE ( 'NONE', *, *, #10308, .T. ) ;
#5839 = CARTESIAN_POINT ( 'NONE',  ( -68.99615306438090556, 77.40823528813029952, -15.00000000000001421 ) ) ;
#5840 = VERTEX_POINT ( 'NONE', #18358 ) ;
#5841 = EDGE_CURVE ( 'NONE', #15702, #3179, #2542, .T. ) ;
#5842 = ORIENTED_EDGE ( 'NONE', *, *, #9586, .F. ) ;
#5843 = EDGE_CURVE ( 'NONE', #2177, #7603, #4726, .T. ) ;
#5844 = EDGE_CURVE ( 'NONE', #17429, #7061, #8245, .T. ) ;
#5845 = AXIS2_PLACEMENT_3D ( 'NONE', #6133, #14839, #17548 ) ;
#5846 = CIRCLE ( 'NONE', #16292, 10.24900000000000055 ) ;
#5847 = EDGE_CURVE ( 'NONE', #7166, #6487, #2436, .T. ) ;
#5848 = ORIENTED_EDGE ( 'NONE', *, *, #233, .T. ) ;
#5849 = FILL_AREA_STYLE ('',( #10511 ) ) ;
#5850 = DIRECTION ( 'NONE',  ( -0.9396926207859157554, 0.3420201433256481738, -4.890320548438487362E-16 ) ) ;
#5851 = CARTESIAN_POINT ( 'NONE',  ( -71.24615306438083451, 97.07672421522921979, -15.00000000000001421 ) ) ;
#5852 = EDGE_CURVE ( 'NONE', #7640, #15247, #9220, .T. ) ;
#5853 = ORIENTED_EDGE ( 'NONE', *, *, #4855, .T. ) ;
#5854 = EDGE_CURVE ( 'NONE', #8416, #12329, #16666, .T. ) ;
#5855 = CARTESIAN_POINT ( 'NONE',  ( -31.74593505105995916, -91.08423613455721579, -10.65431531532567710 ) ) ;
#5856 = LINE ( 'NONE', #4440, #13717 ) ;
#5857 = DIRECTION ( 'NONE',  ( 1.000000000000000000, 0.000000000000000000, 0.000000000000000000 ) ) ;
#5858 = LINE ( 'NONE', #3308, #4898 ) ;
#5859 = VERTEX_POINT ( 'NONE', #5424 ) ;
#5860 = FACE_OUTER_BOUND ( 'NONE', #10082, .T. ) ;
#5861 = DIRECTION ( 'NONE',  ( -0.000000000000000000, 0.000000000000000000, 1.000000000000000000 ) ) ;
#5862 = EDGE_LOOP ( 'NONE', ( #5924, #1837, #1129, #12780 ) ) ;
#5863 = CARTESIAN_POINT ( 'NONE',  ( -71.24615306438100504, 53.09442711522921599, -15.00000000000001421 ) ) ;
#5864 = CARTESIAN_POINT ( 'NONE',  ( -57.08002265617300708, 84.22855780814606419, -47.50000000000000000 ) ) ;
#5865 = ORIENTED_EDGE ( 'NONE', *, *, #9959, .F. ) ;
#5866 = EDGE_CURVE ( 'NONE', #18116, #3203, #8023, .T. ) ;
#5867 = ORIENTED_EDGE ( 'NONE', *, *, #12738, .T. ) ;
#5868 = DIRECTION ( 'NONE',  ( 0.000000000000000000, 0.000000000000000000, 1.000000000000000000 ) ) ;
#5869 = CARTESIAN_POINT ( 'NONE',  ( -64.09025127992788384, 59.14618053571278722, 28.00000000000000355 ) ) ;
#5870 =( NAMED_UNIT ( * ) SI_UNIT ( $, .STERADIAN. ) SOLID_ANGLE_UNIT ( ) );
#5871 = LINE ( 'NONE', #6128, #15012 ) ;
#5872 = FACE_OUTER_BOUND ( 'NONE', #5115, .T. ) ;
#5873 = ORIENTED_EDGE ( 'NONE', *, *, #16015, .F. ) ;
#5874 = DIRECTION ( 'NONE',  ( 0.000000000000000000, 5.551115123125748189E-17, 1.000000000000000000 ) ) ;
#5875 = CARTESIAN_POINT ( 'NONE',  ( -65.72457281170906640, 78.72276507608454210, -167.1454815528550739 ) ) ;
#5876 = CARTESIAN_POINT ( 'NONE',  ( -41.64957301763954689, 53.51189571422416691, 24.86776167054292586 ) ) ;
#5877 = CYLINDRICAL_SURFACE ( 'NONE', #1850, 3.999999999999996447 ) ;
#5878 = EDGE_LOOP ( 'NONE', ( #369, #15220, #5705, #2844 ) ) ;
#5879 = CARTESIAN_POINT ( 'NONE',  ( -68.99615306438111872, 13.96152643166267993, -15.00000000000001421 ) ) ;
#5880 = DIRECTION ( 'NONE',  ( -0.9396926207858996571, 0.3420201433256928603, -4.890320548438403546E-16 ) ) ;
#5881 = VERTEX_POINT ( 'NONE', #4041 ) ;
#5882 = CARTESIAN_POINT ( 'NONE',  ( -47.15582643534892782, 86.78830982163900387, -15.00000000000001421 ) ) ;
#5883 = CARTESIAN_POINT ( 'NONE',  ( 98.04320049944426785, 84.22855780814606419, 62.50000000000001421 ) ) ;
#5884 = ORIENTED_EDGE ( 'NONE', *, *, #17386, .F. ) ;
#5885 = ORIENTED_EDGE ( 'NONE', *, *, #11215, .T. ) ;
#5886 = EDGE_LOOP ( 'NONE', ( #17028, #11122, #6024, #17250 ) ) ;
#5887 = CARTESIAN_POINT ( 'NONE',  ( 0.2573354458087894203, 4.368923434677159712, 5.432802636760818871 ) ) ;
#5888 = DIRECTION ( 'NONE',  ( 0.000000000000000000, 1.000000000000000000, 0.000000000000000000 ) ) ;
#5889 = LINE ( 'NONE', #7312, #10721 ) ;
#5890 = LINE ( 'NONE', #7313, #4196 ) ;
#5891 = LINE ( 'NONE', #7396, #3322 ) ;
#5892 = ORIENTED_EDGE ( 'NONE', *, *, #13149, .T. ) ;
#5893 = ADVANCED_FACE ( 'NONE', ( #2252 ), #16642, .T. ) ;
#5894 = DIRECTION ( 'NONE',  ( 1.000000000000000000, 0.000000000000000000, 3.771137991253934490E-16 ) ) ;
#5895 = DIRECTION ( 'NONE',  ( 0.000000000000000000, 0.000000000000000000, 1.000000000000000000 ) ) ;
#5896 = CARTESIAN_POINT ( 'NONE',  ( -68.99615306438086293, 89.35975003166268493, -15.00000000000001421 ) ) ;
#5897 = ORIENTED_EDGE ( 'NONE', *, *, #1163, .F. ) ;
#5898 = ADVANCED_BREP_SHAPE_REPRESENTATION ( '', ( #152, #16217 ), #12057 ) ;
#5899 = CARTESIAN_POINT ( 'NONE',  ( -46.83322972390671879, 84.01587117655466841, -15.00000000000001421 ) ) ;
#5900 = FACE_OUTER_BOUND ( 'NONE', #16304, .T. ) ;
#5901 = ORIENTED_EDGE ( 'NONE', *, *, #13624, .T. ) ;
#5902 = ORIENTED_EDGE ( 'NONE', *, *, #8710, .T. ) ;
#5903 = DIRECTION ( 'NONE',  ( 1.000000000000000000, 0.000000000000000000, 0.000000000000000000 ) ) ;
#5904 = DIRECTION ( 'NONE',  ( 1.000000000000000000, 0.000000000000000000, 0.000000000000000000 ) ) ;
#5905 = DIRECTION ( 'NONE',  ( 0.000000000000000000, 1.000000000000000000, 0.000000000000000000 ) ) ;
#5906 = EDGE_LOOP ( 'NONE', ( #13535, #18494, #12945, #13795 ) ) ;
#5907 = ORIENTED_EDGE ( 'NONE', *, *, #11454, .T. ) ;
#5908 = VECTOR ( 'NONE', #16484, 1000.000000000000000 ) ;
#5909 = CARTESIAN_POINT ( 'NONE',  ( -68.99615306438072082, 130.2004544816626890, -15.00000000000001421 ) ) ;
#5910 = LINE ( 'NONE', #15935, #933 ) ;
#5911 = DIRECTION ( 'NONE',  ( 1.000000000000000000, 0.000000000000000000, 0.000000000000000000 ) ) ;
#5912 = ADVANCED_FACE ( 'NONE', ( #15150 ), #13952, .T. ) ;
#5913 = LINE ( 'NONE', #11557, #16188 ) ;
#5914 = ORIENTED_EDGE ( 'NONE', *, *, #3780, .T. ) ;
#5915 = LINE ( 'NONE', #5839, #11637 ) ;
#5916 = ORIENTED_EDGE ( 'NONE', *, *, #9268, .F. ) ;
#5917 = VERTEX_POINT ( 'NONE', #1048 ) ;
#5918 = EDGE_CURVE ( 'NONE', #10909, #5337, #12211, .T. ) ;
#5919 = VECTOR ( 'NONE', #7861, 1000.000000000000000 ) ;
#5920 = ORIENTED_EDGE ( 'NONE', *, *, #14208, .T. ) ;
#5921 = CARTESIAN_POINT ( 'NONE',  ( -76.37409655828236055, -111.0842361345572158, -28.18308811886544873 ) ) ;
#5922 = PLANE ( 'NONE',  #1604 ) ;
#5923 = CARTESIAN_POINT ( 'NONE',  ( -92.59262256747318531, 0.3328663868096687350, -25.00000000000000000 ) ) ;
#5924 = ORIENTED_EDGE ( 'NONE', *, *, #6411, .F. ) ;
#5925 = EDGE_CURVE ( 'NONE', #17041, #7723, #2951, .T. ) ;
#5926 = DIRECTION ( 'NONE',  ( 0.000000000000000000, 1.000000000000000000, 0.000000000000000000 ) ) ;
#5927 = CARTESIAN_POINT ( 'NONE',  ( -57.08002265617300708, 84.22855780814606419, 68.73600986863397111 ) ) ;
#5928 = LINE ( 'NONE', #14371, #1817 ) ;
#5929 = ADVANCED_FACE ( 'NONE', ( #15060 ), #13857, .F. ) ;
#5930 = LINE ( 'NONE', #14554, #2846 ) ;
#5931 = EDGE_LOOP ( 'NONE', ( #8368, #7347, #9008, #270, #13047, #12711 ) ) ;
#5932 = ADVANCED_FACE ( 'NONE', ( #18250 ), #12659, .T. ) ;
#5933 = DIRECTION ( 'NONE',  ( 0.000000000000000000, 0.000000000000000000, -1.000000000000000000 ) ) ;
#5934 = VECTOR ( 'NONE', #15699, 1000.000000000000114 ) ;
#5935 = CARTESIAN_POINT ( 'NONE',  ( -75.86129610575210336, 61.64996188551982925, 25.00000000000000355 ) ) ;
#5936 = CARTESIAN_POINT ( 'NONE',  ( -57.74389692835771370, 95.01461175692088545, -15.00000000000001421 ) ) ;
#5937 = ORIENTED_EDGE ( 'NONE', *, *, #11294, .T. ) ;
#5938 = CARTESIAN_POINT ( 'NONE',  ( -77.38579898953899772, 74.98691627113741731, 102.5000000000000000 ) ) ;
#5939 = EDGE_CURVE ( 'NONE', #513, #11655, #10418, .T. ) ;
#5940 = ADVANCED_FACE ( 'NONE', ( #847 ), #13759, .F. ) ;
#5941 = DIRECTION ( 'NONE',  ( 0.000000000000000000, 0.000000000000000000, 1.000000000000000000 ) ) ;
#5942 = EDGE_CURVE ( 'NONE', #14470, #8569, #4217, .T. ) ;
#5943 = VERTEX_POINT ( 'NONE', #3085 ) ;
#5944 = ORIENTED_EDGE ( 'NONE', *, *, #156, .F. ) ;
#5945 = EDGE_CURVE ( 'NONE', #15227, #4300, #14306, .T. ) ;
#5946 = VECTOR ( 'NONE', #4165, 1000.000000000000000 ) ;
#5947 = CARTESIAN_POINT ( 'NONE',  ( -36.77424632280495587, 74.98691627113812785, 97.49999999999998579 ) ) ;
#5948 = EDGE_CURVE ( 'NONE', #8797, #8085, #5701, .T. ) ;
#5949 = AXIS2_PLACEMENT_3D ( 'NONE', #15950, #13145, #17340 ) ;
#5950 = DIRECTION ( 'NONE',  ( 1.000000000000000000, 0.000000000000000000, 0.000000000000000000 ) ) ;
#5951 = CARTESIAN_POINT ( 'NONE',  ( -25.66933353722515676, -96.08423613455721579, 5.654315315325685987 ) ) ;
#5952 = CARTESIAN_POINT ( 'NONE',  ( -66.00585202009862940, 110.5691553257988460, 25.00000000000000355 ) ) ;
#5953 = ORIENTED_EDGE ( 'NONE', *, *, #8507, .F. ) ;
#5954 = LINE ( 'NONE', #12916, #12595 ) ;
#5955 = PLANE ( 'NONE',  #4047 ) ;
#5956 = EDGE_CURVE ( 'NONE', #14934, #3601, #8332, .T. ) ;
#5957 = DIRECTION ( 'NONE',  ( 1.000000000000000000, 0.000000000000000000, 0.000000000000000000 ) ) ;
#5958 = CARTESIAN_POINT ( 'NONE',  ( -127.5926225674731995, 110.5691553257988460, 26.35917033480641436 ) ) ;
#5959 = EDGE_CURVE ( 'NONE', #11545, #15187, #7040, .T. ) ;
#5960 = CARTESIAN_POINT ( 'NONE',  ( -37.41825604777831416, 91.72841893195356988, 62.00367782810642581 ) ) ;
#5961 = DIRECTION ( 'NONE',  ( 0.000000000000000000, 0.000000000000000000, -1.000000000000000000 ) ) ;
#5962 = VECTOR ( 'NONE', #13476, 1000.000000000000000 ) ;
#5963 = VERTEX_POINT ( 'NONE', #7209 ) ;
#5964 = CARTESIAN_POINT ( 'NONE',  ( -25.66933353722515676, -91.08423613455721579, -5.654315315325675328 ) ) ;
#5965 = VECTOR ( 'NONE', #18034, 1000.000000000000000 ) ;
#5966 = ORIENTED_EDGE ( 'NONE', *, *, #2166, .F. ) ;
#5967 = ORIENTED_EDGE ( 'NONE', *, *, #15782, .T. ) ;
#5968 = EDGE_LOOP ( 'NONE', ( #10878, #15428, #1152, #16507 ) ) ;
#5969 = DIRECTION ( 'NONE',  ( 0.9396926207859097602, 0.3420201433256649937, -1.086737899652991371E-16 ) ) ;
#5970 = DIRECTION ( 'NONE',  ( 0.000000000000000000, 0.000000000000000000, 1.000000000000000000 ) ) ;
#5971 = VECTOR ( 'NONE', #2508, 1000.000000000000000 ) ;
#5972 = DIRECTION ( 'NONE',  ( -0.000000000000000000, -0.000000000000000000, 1.000000000000000000 ) ) ;
#5973 = CARTESIAN_POINT ( 'NONE',  ( -64.50972932340006594, 92.07579602767982863, -15.00000000000001421 ) ) ;
#5974 = DIRECTION ( 'NONE',  ( -0.000000000000000000, -0.000000000000000000, -1.000000000000000000 ) ) ;
#5975 = VECTOR ( 'NONE', #16700, 1000.000000000000000 ) ;
#5976 = DIRECTION ( 'NONE',  ( 0.000000000000000000, 1.000000000000000000, 0.000000000000000000 ) ) ;
#5977 = AXIS2_PLACEMENT_3D ( 'NONE', #4660, #17653, #10458 ) ;
#5978 = ORIENTED_EDGE ( 'NONE', *, *, #17822, .F. ) ;
#5979 = DIRECTION ( 'NONE',  ( 0.000000000000000000, 0.000000000000000000, -1.000000000000000000 ) ) ;
#5980 = CARTESIAN_POINT ( 'NONE',  ( -76.63889361118854993, -94.42547395655697073, 44.74949031872077398 ) ) ;
#5981 = DIRECTION ( 'NONE',  ( 0.000000000000000000, 0.000000000000000000, -1.000000000000000000 ) ) ;
#5982 = ORIENTED_EDGE ( 'NONE', *, *, #13255, .F. ) ;
#5983 = LINE ( 'NONE', #7591, #10029 ) ;
#5984 = DIRECTION ( 'NONE',  ( -1.000000000000000000, 0.000000000000000000, 0.000000000000000000 ) ) ;
#5985 = ORIENTED_EDGE ( 'NONE', *, *, #7203, .T. ) ;
#5986 = VECTOR ( 'NONE', #10001, 1000.000000000000000 ) ;
#5987 = AXIS2_PLACEMENT_3D ( 'NONE', #7630, #4905, #13700 ) ;
#5988 = EDGE_CURVE ( 'NONE', #13329, #4697, #10026, .T. ) ;
#5989 = ORIENTED_EDGE ( 'NONE', *, *, #1958, .F. ) ;
#5990 = DIRECTION ( 'NONE',  ( 0.000000000000000000, 1.000000000000000000, -0.000000000000000000 ) ) ;
#5991 = CARTESIAN_POINT ( 'NONE',  ( -66.40868851600845346, 56.38066346224191960, 25.00000000000000355 ) ) ;
#5992 = CARTESIAN_POINT ( 'NONE',  ( -68.99615306438072082, 133.3420471316626958, -15.00000000000001421 ) ) ;
#5993 = ORIENTED_EDGE ( 'NONE', *, *, #4981, .F. ) ;
#5994 = EDGE_CURVE ( 'NONE', #3227, #9065, #7122, .T. ) ;
#5995 = AXIS2_PLACEMENT_3D ( 'NONE', #2861, #4424, #13056 ) ;
#5996 = ORIENTED_EDGE ( 'NONE', *, *, #6268, .T. ) ;
#5997 = DIRECTION ( 'NONE',  ( 1.156482317317869999E-16, 0.000000000000000000, 1.000000000000000000 ) ) ;
#5998 = CARTESIAN_POINT ( 'NONE',  ( 0.05533025579370332708, -6.264553569211981809, 2.149474931388166699 ) ) ;
#5999 = CARTESIAN_POINT ( 'NONE',  ( -123.4618227840623632, -151.5628872026273086, 36.00000000000001421 ) ) ;
#6001 = B_SPLINE_CURVE_WITH_KNOTS ( 'NONE', 3,
 ( #13043, #121, #2744, #4237, #2930, #212, #5636, #7141, #12855, #8453, #8557, #11357, #17049, #3019, #1615, #10216, #9949, #24, #7403, #5727 ),
 .UNSPECIFIED., .F., .F.,
 ( 4, 2, 2, 2, 2, 2, 2, 2, 2, 4 ),
 ( 0.000000000000000000, 0.001278592738658804314, 0.002557185477317608629, 0.003835778215976412726, 0.005114370954635217258, 0.006392963693294019187, 0.007671556431952822851, 0.008950149170611624780, 0.009589445539941010566, 0.01022874190927039288 ),
 .UNSPECIFIED. ) ;
#6000 = CARTESIAN_POINT ( 'NONE',  ( 103.5381772159376084, -111.0842361345572158, -36.00000000000000000 ) ) ;
#6002 = VECTOR ( 'NONE', #778, 1000.000000000000000 ) ;
#6003 = ORIENTED_EDGE ( 'NONE', *, *, #4260, .T. ) ;
#6004 = FACE_OUTER_BOUND ( 'NONE', #4341, .T. ) ;
#6005 = ORIENTED_EDGE ( 'NONE', *, *, #9042, .T. ) ;
#6006 = CARTESIAN_POINT ( 'NONE',  ( -97.59262256747317110, 0.3328663868096687350, 25.00000000000000000 ) ) ;
#6007 = ORIENTED_EDGE ( 'NONE', *, *, #4891, .F. ) ;
#6008 = AXIS2_PLACEMENT_3D ( 'NONE', #859, #9377, #15076 ) ;
#6009 = ORIENTED_EDGE ( 'NONE', *, *, #1497, .F. ) ;
#6010 = AXIS2_PLACEMENT_3D ( 'NONE', #14293, #6807, #12528 ) ;
#6011 = CIRCLE ( 'NONE', #2440, 12.29357405616490695 ) ;
#6012 = CARTESIAN_POINT ( 'NONE',  ( -66.63376473465912397, -19.34983604512935429, 57.00000000000000000 ) ) ;
#6013 = CARTESIAN_POINT ( 'NONE',  ( -107.5676225674731654, 57.88796029049330372, 22.35917033480641791 ) ) ;
#6014 = ORIENTED_EDGE ( 'NONE', *, *, #4360, .F. ) ;
#6015 = CARTESIAN_POINT ( 'NONE',  ( -64.50972932340006594, 92.07579602767982863, 15.00000000000006928 ) ) ;
#6016 = DIRECTION ( 'NONE',  ( 0.000000000000000000, 1.000000000000000000, 0.000000000000000000 ) ) ;
#6017 = LINE ( 'NONE', #16120, #14195 ) ;
#6018 = ORIENTED_EDGE ( 'NONE', *, *, #4803, .T. ) ;
#6019 = VECTOR ( 'NONE', #5305, 1000.000000000000000 ) ;
#6020 = EDGE_CURVE ( 'NONE', #9668, #1526, #13101, .T. ) ;
#6021 = DIRECTION ( 'NONE',  ( 1.000000000000000000, 0.000000000000000000, 0.000000000000000000 ) ) ;
#6022 = DIRECTION ( 'NONE',  ( 1.000000000000000000, 0.000000000000000000, 3.771137991253934490E-16 ) ) ;
#6023 = CARTESIAN_POINT ( 'NONE',  ( -49.58002265617300708, 84.22855780814606419, -35.00000000000000000 ) ) ;
#6024 = ORIENTED_EDGE ( 'NONE', *, *, #13278, .T. ) ;
#6025 = AXIS2_PLACEMENT_3D ( 'NONE', #12627, #18325, #5306 ) ;
#6026 = AXIS2_PLACEMENT_3D ( 'NONE', #1854, #18109, #3249 ) ;
#6027 = CARTESIAN_POINT ( 'NONE',  ( -97.59262256747319952, 117.8748711238780373, 25.00000000000000000 ) ) ;
#6028 = DIRECTION ( 'NONE',  ( 0.000000000000000000, 1.000000000000000000, -0.000000000000000000 ) ) ;
#6029 = ORIENTED_EDGE ( 'NONE', *, *, #12602, .F. ) ;
#6030 = EDGE_CURVE ( 'NONE', #15808, #2407, #5531, .T. ) ;
#6031 = EDGE_LOOP ( 'NONE', ( #9202, #1331 ) ) ;
#6032 = TOROIDAL_SURFACE ( 'NONE', #15000, 40.40389983439752086, 5.000000000000000000 ) ;
#6033 = ORIENTED_EDGE ( 'NONE', *, *, #7916, .F. ) ;
#6034 = CARTESIAN_POINT ( 'NONE',  ( -106.3193689061042164, 112.6569076202650450, 97.49999999999998579 ) ) ;
#6035 = CIRCLE ( 'NONE', #11148, 4.025000000000000355 ) ;
#6036 = VECTOR ( 'NONE', #14614, 1000.000000000000000 ) ;
#6037 = DIRECTION ( 'NONE',  ( 0.000000000000000000, 0.000000000000000000, 1.000000000000000000 ) ) ;
#6038 = CARTESIAN_POINT ( 'NONE',  ( -40.83486628351231218, 66.64375664990294013, 92.50000000000000000 ) ) ;
#6039 = FACE_OUTER_BOUND ( 'NONE', #11449, .T. ) ;
#6040 = EDGE_LOOP ( 'NONE', ( #12638, #17797, #2761, #15551 ) ) ;
#6041 = EDGE_CURVE ( 'NONE', #12790, #9020, #12757, .T. ) ;
#6042 = EDGE_CURVE ( 'NONE', #5163, #10938, #18450, .T. ) ;
#6043 = CARTESIAN_POINT ( 'NONE',  ( -71.24615306438086293, 93.93513156522925556, -15.00000000000001421 ) ) ;
#6044 = CYLINDRICAL_SURFACE ( 'NONE', #15092, 71.86696747278378439 ) ;
#6045 = DIRECTION ( 'NONE',  ( 0.000000000000000000, 0.000000000000000000, 1.000000000000000000 ) ) ;
#6046 = LINE ( 'NONE', #16147, #72 ) ;
#6047 = CARTESIAN_POINT ( 'NONE',  ( -36.20358435058752633, 86.88560906486404178, 55.48211817979245808 ) ) ;
#6048 = CIRCLE ( 'NONE', #18330, 7.500000000000000000 ) ;
#6049 = CARTESIAN_POINT ( 'NONE',  ( 124.5381772159375942, -111.0842361345572158, -36.00000000000000000 ) ) ;
#6050 = ORIENTED_EDGE ( 'NONE', *, *, #14387, .F. ) ;
#6051 = EDGE_CURVE ( 'NONE', #6455, #14401, #17123, .T. ) ;
#6052 = CIRCLE ( 'NONE', #12347, 3.999999999999989786 ) ;
#6053 = CARTESIAN_POINT ( 'NONE',  ( -68.99615306438072082, 140.2400882881302948, 15.00000000000006928 ) ) ;
#6054 = CIRCLE ( 'NONE', #15927, 0.4000000000000001887 ) ;
#6055 = DIRECTION ( 'NONE',  ( -0.000000000000000000, -1.000000000000000000, -0.000000000000000000 ) ) ;
#6056 = ORIENTED_EDGE ( 'NONE', *, *, #6283, .T. ) ;
#6057 = AXIS2_PLACEMENT_3D ( 'NONE', #11996, #12100, #13682 ) ;
#6058 = EDGE_CURVE ( 'NONE', #17079, #17041, #11333, .T. ) ;
#6059 = ORIENTED_EDGE ( 'NONE', *, *, #2414, .T. ) ;
#6060 = EDGE_CURVE ( 'NONE', #1931, #6195, #13461, .T. ) ;
#6061 = EDGE_CURVE ( 'NONE', #6521, #13576, #2916, .T. ) ;
#6062 = CIRCLE ( 'NONE', #1014, 4.599999999999992539 ) ;
#6063 = ORIENTED_EDGE ( 'NONE', *, *, #15594, .T. ) ;
#6064 = CARTESIAN_POINT ( 'NONE',  ( 0.000000000000000000, -5.629165124598954684, 3.250000000000013323 ) ) ;
#6065 = CARTESIAN_POINT ( 'NONE',  ( 5.233202738124664855, -19.34983604512936495, -54.79921157549230770 ) ) ;
#6066 = CARTESIAN_POINT ( 'NONE',  ( -78.12361985383351737, 83.98232705807352261, 55.00000000000002842 ) ) ;
#6067 = LINE ( 'NONE', #4669, #11499 ) ;
#6068 = EDGE_CURVE ( 'NONE', #7201, #8164, #8619, .T. ) ;
#6069 = DIRECTION ( 'NONE',  ( -1.000000000000000000, 0.000000000000000000, 0.000000000000000000 ) ) ;
#6070 = AXIS2_PLACEMENT_3D ( 'NONE', #6497, #12216, #10814 ) ;
#6071 = CARTESIAN_POINT ( 'NONE',  ( -60.06546592763127990, -96.08423613455721579, -2.420256967240809069E-13 ) ) ;
#6072 = FACE_OUTER_BOUND ( 'NONE', #16035, .T. ) ;
#6073 = ORIENTED_EDGE ( 'NONE', *, *, #1762, .T. ) ;
#6074 = LINE ( 'NONE', #8817, #17955 ) ;
#6075 = CARTESIAN_POINT ( 'NONE',  ( -76.42964172313227778, -95.23217669033336108, 44.98760873426157758 ) ) ;
#6076 = CARTESIAN_POINT ( 'NONE',  ( -123.4618227840623632, -111.0842361345572158, 57.00000000000000000 ) ) ;
#6077 = ORIENTED_EDGE ( 'NONE', *, *, #1612, .F. ) ;
#6078 = LINE ( 'NONE', #17403, #1941 ) ;
#6079 = CARTESIAN_POINT ( 'NONE',  ( -57.08002265617300708, 84.22855780814606419, 37.50000000000000000 ) ) ;
#6080 = ORIENTED_EDGE ( 'NONE', *, *, #5675, .F. ) ;
#6081 = VECTOR ( 'NONE', #8688, 1000.000000000000000 ) ;
#6082 = AXIS2_PLACEMENT_3D ( 'NONE', #1441, #32, #14446 ) ;
#6083 = VERTEX_POINT ( 'NONE', #17025 ) ;
#6084 = CARTESIAN_POINT ( 'NONE',  ( -70.71978124295696944, -96.08423613455721579, 5.204170427930421283E-15 ) ) ;
#6085 = CARTESIAN_POINT ( 'NONE',  ( -57.89103256796045116, 73.45256821284057480, 15.00000000000006928 ) ) ;
#6086 = LINE ( 'NONE', #2852, #9952 ) ;
#6087 = ORIENTED_EDGE ( 'NONE', *, *, #17595, .F. ) ;
#6088 = CARTESIAN_POINT ( 'NONE',  ( -27.58560781757364211, -92.35432432510553724, 7.309979984196399272 ) ) ;
#6089 = VERTEX_POINT ( 'NONE', #2996 ) ;
#6090 = CIRCLE ( 'NONE', #18376, 26.04359719766049608 ) ;
#6091 = DIRECTION ( 'NONE',  ( -1.000000000000000000, -3.016910393003138520E-15, 0.000000000000000000 ) ) ;
#6092 = CARTESIAN_POINT ( 'NONE',  ( -60.06546592763129411, -96.08423613455721579, -6.292668114826103378E-13 ) ) ;
#6093 = LINE ( 'NONE', #8845, #16252 ) ;
#6094 = CYLINDRICAL_SURFACE ( 'NONE', #3959, 11.04359719766049430 ) ;
#6095 = VECTOR ( 'NONE', #3783, 1000.000000000000114 ) ;
#6096 = EDGE_LOOP ( 'NONE', ( #11888, #16382 ) ) ;
#6097 = VECTOR ( 'NONE', #3352, 1000.000000000000000 ) ;
#6098 = CARTESIAN_POINT ( 'NONE',  ( -68.99615306438117557, 1.395155831662692192, -167.1454815528550739 ) ) ;
#6099 = ORIENTED_EDGE ( 'NONE', *, *, #14208, .F. ) ;
#6100 = CARTESIAN_POINT ( 'NONE',  ( -68.99615306438106188, 24.00116023813026445, -167.1454815528550739 ) ) ;
#6101 = ORIENTED_EDGE ( 'NONE', *, *, #4788, .T. ) ;
#6102 = ORIENTED_EDGE ( 'NONE', *, *, #18204, .F. ) ;
#6103 = AXIS2_PLACEMENT_3D ( 'NONE', #2507, #9613, #15315 ) ;
#6104 = VECTOR ( 'NONE', #8694, 1000.000000000000000 ) ;
#6105 = VECTOR ( 'NONE', #8423, 1000.000000000000000 ) ;
#6106 = DIRECTION ( 'NONE',  ( 0.000000000000000000, 1.000000000000000000, 0.000000000000000000 ) ) ;
#6107 = FACE_OUTER_BOUND ( 'NONE', #7738, .T. ) ;
#6108 = CARTESIAN_POINT ( 'NONE',  ( -71.24615306438067819, 145.0894847045637732, -167.1454815528550739 ) ) ;
#6109 = VERTEX_POINT ( 'NONE', #8706 ) ;
#6110 = DIRECTION ( 'NONE',  ( 0.000000000000000000, 0.000000000000000000, -1.000000000000000000 ) ) ;
#6111 = DIRECTION ( 'NONE',  ( 1.000000000000000000, 0.000000000000000000, 0.000000000000000000 ) ) ;
#6112 = CARTESIAN_POINT ( 'NONE',  ( -56.41614838398844256, 95.01461175692088545, -15.00000000000001421 ) ) ;
#6113 = ORIENTED_EDGE ( 'NONE', *, *, #4582, .F. ) ;
#6114 = FACE_OUTER_BOUND ( 'NONE', #5581, .T. ) ;
#6115 = CARTESIAN_POINT ( 'NONE',  ( -57.08002265617300708, 84.22855780814606419, -28.00000000000000355 ) ) ;
#6116 = DIRECTION ( 'NONE',  ( 0.000000000000000000, 0.000000000000000000, 1.000000000000000000 ) ) ;
#6118 = ORIENTED_EDGE ( 'NONE', *, *, #10335, .T. ) ;
#6117 = EDGE_CURVE ( 'NONE', #12880, #3167, #8386, .T. ) ;
#6119 = CONICAL_SURFACE ( 'NONE', #16585, 12.29357405616490695, 0.1302312384721128480 ) ;
#6120 = FACE_OUTER_BOUND ( 'NONE', #6307, .T. ) ;
#6121 = CARTESIAN_POINT ( 'NONE',  ( -42.53669312409158465, -91.08423613455721579, 5.204170427930421283E-15 ) ) ;
#6122 = EDGE_LOOP ( 'NONE', ( #16734, #1983, #2667, #5516 ) ) ;
#6123 = ORIENTED_EDGE ( 'NONE', *, *, #7992, .T. ) ;
#6124 = ORIENTED_EDGE ( 'NONE', *, *, #17608, .T. ) ;
#6125 = CARTESIAN_POINT ( 'NONE',  ( -71.24615306438120399, -0.3126479347707322720, -15.00000000000001421 ) ) ;
#6126 = CARTESIAN_POINT ( 'NONE',  ( 0.000000000000000000, 0.000000000000000000, 0.000000000000000000 ) ) ;
#6127 = CARTESIAN_POINT ( 'NONE',  ( -68.99615306438106188, 27.14275288813031040, 15.00000000000006928 ) ) ;
#6128 = CARTESIAN_POINT ( 'NONE',  ( -60.06546592763127990, -91.08423613455721579, -2.420256967240809069E-13 ) ) ;
#6129 = LINE ( 'NONE', #13441, #12984 ) ;
#6130 = ORIENTED_EDGE ( 'NONE', *, *, #12728, .F. ) ;
#6131 = PLANE ( 'NONE',  #294 ) ;
#6132 = DIRECTION ( 'NONE',  ( -1.000000000000000000, 0.000000000000000000, 0.000000000000000000 ) ) ;
#6133 = CARTESIAN_POINT ( 'NONE',  ( -67.79562744116532258, 82.83016482797231106, -15.00000000000001421 ) ) ;
#6134 = CARTESIAN_POINT ( 'NONE',  ( -127.5926225674731995, 106.8071537307722991, 25.00000000000000355 ) ) ;
#6135 = DIRECTION ( 'NONE',  ( 1.000000000000000000, 0.000000000000000000, 3.771137991253934490E-16 ) ) ;
#6136 = ORIENTED_EDGE ( 'NONE', *, *, #10317, .T. ) ;
#6137 = DIRECTION ( 'NONE',  ( 1.000000000000000000, 0.000000000000000000, 0.000000000000000000 ) ) ;
#6138 = VERTEX_POINT ( 'NONE', #1502 ) ;
#6139 = LINE ( 'NONE', #16259, #17934 ) ;
#6140 = CARTESIAN_POINT ( 'NONE',  ( -49.93060289285580922, 91.57211267264388255, -167.1454815528550739 ) ) ;
#6141 = ORIENTED_EDGE ( 'NONE', *, *, #8798, .T. ) ;
#6142 = ORIENTED_EDGE ( 'NONE', *, *, #3410, .F. ) ;
#6143 = EDGE_CURVE ( 'NONE', #2924, #3192, #4126, .T. ) ;
#6144 = MANIFOLD_SOLID_BREP ( 'Boss-Extrude16', #132 ) ;
#6145 = EDGE_CURVE ( 'NONE', #8271, #3955, #14645, .T. ) ;
#6146 = ORIENTED_EDGE ( 'NONE', *, *, #14984, .F. ) ;
#6147 = CYLINDRICAL_SURFACE ( 'NONE', #15693, 7.500000000000000000 ) ;
#6148 = CARTESIAN_POINT ( 'NONE',  ( -92.59262256747321373, 107.8748711238780373, 35.00000000000000000 ) ) ;
#6149 = DIRECTION ( 'NONE',  ( -0.9396926207859084279, 0.3420201433256686574, -4.890320548438448905E-16 ) ) ;
#6150 = DIRECTION ( 'NONE',  ( 0.9396926207859084279, 0.3420201433256686574, 0.000000000000000000 ) ) ;
#6151 = DIRECTION ( 'NONE',  ( -0.9999883591161159435, 0.004825104377941397994, 0.000000000000000000 ) ) ;
#6152 = EDGE_CURVE ( 'NONE', #17871, #5721, #13363, .T. ) ;
#6153 = DIRECTION ( 'NONE',  ( 0.000000000000000000, 0.000000000000000000, 1.000000000000000000 ) ) ;
#6154 = LINE ( 'NONE', #6447, #11714 ) ;
#6155 = EDGE_LOOP ( 'NONE', ( #7487, #3511, #15396, #4014 ) ) ;
#6156 = EDGE_CURVE ( 'NONE', #17891, #8485, #16436, .T. ) ;
#6157 = EDGE_CURVE ( 'NONE', #15640, #10340, #13456, .T. ) ;
#6158 = FACE_OUTER_BOUND ( 'NONE', #15357, .T. ) ;
#6159 = CARTESIAN_POINT ( 'NONE',  ( -68.99615306438086293, 92.50134268166266338, 15.00000000000006928 ) ) ;
#6160 = DIRECTION ( 'NONE',  ( 1.000000000000000000, 0.000000000000000000, 0.000000000000000000 ) ) ;
#6161 = ORIENTED_EDGE ( 'NONE', *, *, #9126, .F. ) ;
#6162 = CARTESIAN_POINT ( 'NONE',  ( -68.99615306438072082, 130.8153103381302742, 15.00000000000006928 ) ) ;
#6163 = CARTESIAN_POINT ( 'NONE',  ( -68.99615306438074924, 121.3905323881302962, 15.00000000000006928 ) ) ;
#6164 = ORIENTED_EDGE ( 'NONE', *, *, #11353, .F. ) ;
#6165 = EDGE_CURVE ( 'NONE', #15625, #8437, #17558, .T. ) ;
#6166 = EDGE_CURVE ( 'NONE', #15968, #9281, #17654, .T. ) ;
#6167 = EDGE_CURVE ( 'NONE', #4375, #7124, #10657, .T. ) ;
#6168 = ORIENTED_EDGE ( 'NONE', *, *, #3002, .F. ) ;
#6169 = EDGE_CURVE ( 'NONE', #4644, #9204, #2038, .T. ) ;
#6170 = CARTESIAN_POINT ( 'NONE',  ( -68.99615306438111872, 10.81993378166265529, -15.00000000000001421 ) ) ;
#6171 = CARTESIAN_POINT ( 'NONE',  ( 98.04320049944426785, 94.60860137538374204, 62.50000000000001421 ) ) ;
#6172 = CARTESIAN_POINT ( 'NONE',  ( -38.09490121289055509, 73.26749283227019305, 97.49999999999998579 ) ) ;
#6173 = ORIENTED_EDGE ( 'NONE', *, *, #1176, .F. ) ;
#6174 = LINE ( 'NONE', #6463, #13482 ) ;
#6175 = EDGE_LOOP ( 'NONE', ( #9524, #4043, #495, #463 ) ) ;
#6176 = CARTESIAN_POINT ( 'NONE',  ( -67.59262256747319952, 106.8071537307723133, 25.00000000000000355 ) ) ;
#6177 = LINE ( 'NONE', #7786, #12300 ) ;
#6178 = CARTESIAN_POINT ( 'NONE',  ( -77.53403837096536222, 89.18782894963362651, 56.85235929646029263 ) ) ;
#6179 = LINE ( 'NONE', #224, #16804 ) ;
#6180 = ORIENTED_EDGE ( 'NONE', *, *, #2156, .F. ) ;
#6181 = EDGE_CURVE ( 'NONE', #3203, #2791, #1799, .T. ) ;
#6182 = ADVANCED_FACE ( 'NONE', ( #2132 ), #4499, .T. ) ;
#6183 = CARTESIAN_POINT ( 'NONE',  ( -71.24615306438070661, 141.0590213152292449, -167.1454815528550739 ) ) ;
#6184 = VERTEX_POINT ( 'NONE', #15987 ) ;
#6185 = DIRECTION ( 'NONE',  ( -0.9396926207859097602, 0.3420201433256649937, 1.086737899652991371E-16 ) ) ;
#6186 = ORIENTED_EDGE ( 'NONE', *, *, #2283, .T. ) ;
#6187 = ORIENTED_EDGE ( 'NONE', *, *, #8118, .T. ) ;
#6188 = APPLICATION_CONTEXT ( 'automotive_design' ) ;
#6189 = ORIENTED_EDGE ( 'NONE', *, *, #12899, .F. ) ;
#6190 = DIRECTION ( 'NONE',  ( 0.000000000000000000, 1.000000000000000000, 0.000000000000000000 ) ) ;
#6191 = TOROIDAL_SURFACE ( 'NONE', #8622, 21.04359719766050674, 1.000000000000000000 ) ;
#6192 = FACE_OUTER_BOUND ( 'NONE', #15828, .T. ) ;
#6193 = VERTEX_POINT ( 'NONE', #9242 ) ;
#6194 = CARTESIAN_POINT ( 'NONE',  ( -71.24615306438103346, 46.81124181522922356, -167.1454815528550739 ) ) ;
#6195 = VERTEX_POINT ( 'NONE', #16064 ) ;
#6196 = EDGE_CURVE ( 'NONE', #8556, #1000, #5397, .T. ) ;
#6197 = DIRECTION ( 'NONE',  ( 0.3420201433256649937, 0.9396926207859097602, -0.000000000000000000 ) ) ;
#6198 = ORIENTED_EDGE ( 'NONE', *, *, #17757, .T. ) ;
#6199 = CARTESIAN_POINT ( 'NONE',  ( -57.08002265617300708, 84.22855780814606419, 37.50000000000000000 ) ) ;
#6200 = DIRECTION ( 'NONE',  ( 1.000000000000000000, 0.000000000000000000, 0.000000000000000000 ) ) ;
#6201 = ORIENTED_EDGE ( 'NONE', *, *, #1942, .T. ) ;
#6202 = CARTESIAN_POINT ( 'NONE',  ( -67.59262256747319952, 111.6514400295689171, -22.50837044127971254 ) ) ;
#6203 = VECTOR ( 'NONE', #14409, 999.9999999999998863 ) ;
#6204 = DIRECTION ( 'NONE',  ( 0.000000000000000000, -0.000000000000000000, 1.000000000000000000 ) ) ;
#6205 = ORIENTED_EDGE ( 'NONE', *, *, #9770, .F. ) ;
#6206 = ORIENTED_EDGE ( 'NONE', *, *, #15548, .T. ) ;
#6207 = PRODUCT ( 'C-Frame Forged Steel Casing', 'C-Frame Forged Steel Casing', '', ( #6575 ) ) ;
#6208 = ORIENTED_EDGE ( 'NONE', *, *, #17853, .T. ) ;
#6210 = EDGE_CURVE ( 'NONE', #5095, #10198, #7470, .T. ) ;
#6209 = LINE ( 'NONE', #6496, #8497 ) ;
#6211 = CARTESIAN_POINT ( 'NONE',  ( -71.24615306438089135, 81.36876096522922808, -167.1454815528550739 ) ) ;
#6212 = B_SPLINE_CURVE_WITH_KNOTS ( 'NONE', 3,
 ( #5515, #11240, #2904, #5783, #10096, #16925, #12748, #14393, #1408, #12646, #18344, #8419, #15624, #13008, #18435, #12817, #184, #4114, #9818, #14130 ),
 .UNSPECIFIED., .F., .F.,
 ( 4, 2, 2, 2, 2, 2, 2, 2, 2, 4 ),
 ( -1.439925654488655154E-05, 0.0006244272253376482703, 0.001263253707220183229, 0.002540906670985252497, 0.003818559634750321331, 0.005096212598515389297, 0.006373865562280459432, 0.007651518526045526965, 0.008929171489810596232, 0.01020682445357566463 ),
 .UNSPECIFIED. ) ;
#6213 = EDGE_LOOP ( 'NONE', ( #15633, #15761, #17600, #16394, #5901, #9185, #6243, #14935 ) ) ;
#6214 = DIRECTION ( 'NONE',  ( 0.000000000000000000, 0.000000000000000000, 1.000000000000000000 ) ) ;
#6215 =( LENGTH_UNIT ( ) NAMED_UNIT ( * ) SI_UNIT ( .MILLI., .METRE. ) );
#6216 = DIRECTION ( 'NONE',  ( -4.029365176583844474E-15, 0.000000000000000000, 1.000000000000000000 ) ) ;
#6217 = CIRCLE ( 'NONE', #14896, 4.599999999999999645 ) ;
#6218 = CARTESIAN_POINT ( 'NONE',  ( -55.10846673861666289, 96.57209730311868157, -167.1454815528550739 ) ) ;
#6219 = VERTEX_POINT ( 'NONE', #17475 ) ;
#6220 = EDGE_CURVE ( 'NONE', #8703, #7660, #1978, .T. ) ;
#6221 = FACE_OUTER_BOUND ( 'NONE', #767, .T. ) ;
#6222 = DIRECTION ( 'NONE',  ( -0.000000000000000000, -0.000000000000000000, -1.000000000000000000 ) ) ;
#6223 = LINE ( 'NONE', #531, #13924 ) ;
#6224 = CARTESIAN_POINT ( 'NONE',  ( -70.71978124295696944, -96.08423613455721579, 5.204170427930421283E-15 ) ) ;
#6225 = DIRECTION ( 'NONE',  ( 0.000000000000000000, 1.000000000000000000, 0.000000000000000000 ) ) ;
#6226 = ORIENTED_EDGE ( 'NONE', *, *, #8510, .T. ) ;
#6227 = CARTESIAN_POINT ( 'NONE',  ( -68.99615306438111872, 20.24471173166267235, 15.00000000000006928 ) ) ;
#6228 = DIRECTION ( 'NONE',  ( -0.000000000000000000, 1.200240087506842815E-16, 1.000000000000000000 ) ) ;
#6229 = ORIENTED_EDGE ( 'NONE', *, *, #8997, .F. ) ;
#6230 = CARTESIAN_POINT ( 'NONE',  ( -66.00585202009801833, 57.88796029049324687, 25.00000000000000355 ) ) ;
#6231 = ORIENTED_EDGE ( 'NONE', *, *, #311, .F. ) ;
#6232 = AXIS2_PLACEMENT_3D ( 'NONE', #13998, #11288, #11193 ) ;
#6233 = ORIENTED_EDGE ( 'NONE', *, *, #5821, .F. ) ;
#6234 = VECTOR ( 'NONE', #14380, 1000.000000000000000 ) ;
#6235 = MANIFOLD_SOLID_BREP ( 'Cut-Extrude9', #7289 ) ;
#6236 = ORIENTED_EDGE ( 'NONE', *, *, #13469, .T. ) ;
#6237 = DIRECTION ( 'NONE',  ( -0.000000000000000000, -0.000000000000000000, 1.000000000000000000 ) ) ;
#6238 = DIRECTION ( 'NONE',  ( 0.9396926207859171987, 0.3420201433256444545, 0.000000000000000000 ) ) ;
#6239 = FACE_BOUND ( 'NONE', #11509, .T. ) ;
#6240 = DIRECTION ( 'NONE',  ( 0.000000000000000000, 1.000000000000000000, 0.000000000000000000 ) ) ;
#6241 = CARTESIAN_POINT ( 'NONE',  ( -47.88253357122329845, 84.22855780814606419, 77.50000000000000000 ) ) ;
#6242 = DIRECTION ( 'NONE',  ( 1.000000000000000000, 0.000000000000000000, 0.000000000000000000 ) ) ;
#6243 = ORIENTED_EDGE ( 'NONE', *, *, #17224, .F. ) ;
#6244 = CIRCLE ( 'NONE', #16119, 4.600000000000006750 ) ;
#6245 = DIRECTION ( 'NONE',  ( 0.000000000000000000, -5.551115123125747573E-17, -1.000000000000000000 ) ) ;
#6246 = ADVANCED_FACE ( 'NONE', ( #1021 ), #11129, .F. ) ;
#6247 = DIRECTION ( 'NONE',  ( -1.000000000000000000, 0.000000000000000000, -0.000000000000000000 ) ) ;
#6248 = VECTOR ( 'NONE', #4876, 1000.000000000000000 ) ;
#6249 = DIRECTION ( 'NONE',  ( -0.9396926207859084279, 0.3420201433256686574, 0.000000000000000000 ) ) ;
#6250 = EDGE_LOOP ( 'NONE', ( #15771, #4042, #14803, #10765 ) ) ;
#6251 = FACE_OUTER_BOUND ( 'NONE', #14691, .T. ) ;
#6252 = CARTESIAN_POINT ( 'NONE',  ( -67.59262256747317110, 56.80567558672318995, 22.50837044127973030 ) ) ;
#6253 = ORIENTED_EDGE ( 'NONE', *, *, #14755, .T. ) ;
#6255 = EDGE_CURVE ( 'NONE', #11356, #1931, #8405, .T. ) ;
#6254 = AXIS2_PLACEMENT_3D ( 'NONE', #16576, #12571, #3855 ) ;
#6256 = ORIENTED_EDGE ( 'NONE', *, *, #4083, .F. ) ;
#6257 = PRODUCT_DEFINITION_CONTEXT ( 'detailed design', #11001, 'design' ) ;
#6258 = EDGE_CURVE ( 'NONE', #10059, #1357, #8596, .T. ) ;
#6259 = CIRCLE ( 'NONE', #5977, 4.599999999999999645 ) ;
#6260 = DIRECTION ( 'NONE',  ( 0.000000000000000000, 0.000000000000000000, 1.000000000000000000 ) ) ;
#6261 = CARTESIAN_POINT ( 'NONE',  ( -65.06546592763082515, -111.0842361345572158, -45.05044770573174873 ) ) ;
#6262 = DIRECTION ( 'NONE',  ( -1.000000000000000000, 0.000000000000000000, -0.000000000000000000 ) ) ;
#6263 = CARTESIAN_POINT ( 'NONE',  ( -107.5926225674731853, 110.5691553257988460, -22.33417033480641223 ) ) ;
#6264 = ORIENTED_EDGE ( 'NONE', *, *, #11684, .F. ) ;
#6265 = CARTESIAN_POINT ( 'NONE',  ( -71.24615306438110451, 6.859408104563811115, 15.00000000000006928 ) ) ;
#6266 = DIRECTION ( 'NONE',  ( 0.3420201433256686574, 0.9396926207859084279, -0.000000000000000000 ) ) ;
#6267 = VERTEX_POINT ( 'NONE', #14383 ) ;
#6268 = EDGE_CURVE ( 'NONE', #4518, #13839, #8676, .T. ) ;
#6269 = PLANE ( 'NONE',  #12900 ) ;
#6270 = DIRECTION ( 'NONE',  ( 1.000000000000000000, 0.000000000000000000, 0.000000000000000000 ) ) ;
#6271 = CARTESIAN_POINT ( 'NONE',  ( -78.08890555966455338, 85.46113186790836380, 55.09782012572272691 ) ) ;
#6272 = VECTOR ( 'NONE', #5774, 1000.000000000000000 ) ;
#6273 = EDGE_CURVE ( 'NONE', #5132, #11466, #7183, .T. ) ;
#6274 = CARTESIAN_POINT ( 'NONE',  ( -71.24615306438077766, 97.96559495456378386, 15.00000000000006928 ) ) ;
#6275 = EDGE_LOOP ( 'NONE', ( #3578, #2316, #241, #1008, #15196, #503 ) ) ;
#6276 = VECTOR ( 'NONE', #5609, 1000.000000000000000 ) ;
#6277 = CARTESIAN_POINT ( 'NONE',  ( -68.99615306438109030, 17.71797493813028268, -15.00000000000001421 ) ) ;
#6278 = VERTEX_POINT ( 'NONE', #4380 ) ;
#6279 = VECTOR ( 'NONE', #8208, 1000.000000000000000 ) ;
#6280 = LINE ( 'NONE', #14894, #14874 ) ;
#6281 = ORIENTED_EDGE ( 'NONE', *, *, #2248, .F. ) ;
#6282 = VECTOR ( 'NONE', #10086, 1000.000000000000000 ) ;
#6283 = EDGE_CURVE ( 'NONE', #3665, #7505, #17924, .T. ) ;
#6284 = EDGE_CURVE ( 'NONE', #2737, #10339, #2970, .T. ) ;
#6285 = VERTEX_POINT ( 'NONE', #11503 ) ;
#6286 = TOROIDAL_SURFACE ( 'NONE', #36, 47.49926016645015636, 5.000000000000000000 ) ;
#6287 = EDGE_CURVE ( 'NONE', #11552, #15616, #9907, .T. ) ;
#6288 = DIRECTION ( 'NONE',  ( 0.000000000000000000, 0.000000000000000000, 1.000000000000000000 ) ) ;
#6289 = EDGE_CURVE ( 'NONE', #18359, #17247, #17195, .T. ) ;
#6290 = VERTEX_POINT ( 'NONE', #1207 ) ;
#6291 = AXIS2_PLACEMENT_3D ( 'NONE', #17618, #17530, #14723 ) ;
#6292 = FACE_OUTER_BOUND ( 'NONE', #14862, .T. ) ;
#6293 = DIRECTION ( 'NONE',  ( 1.000000000000000000, 0.000000000000000000, 0.000000000000000000 ) ) ;
#6294 = ORIENTED_EDGE ( 'NONE', *, *, #3204, .T. ) ;
#6295 = EDGE_CURVE ( 'NONE', #9316, #3236, #11313, .T. ) ;
#6296 = CARTESIAN_POINT ( 'NONE',  ( -65.06546592763082515, -96.08423613455721579, -45.05044770573174873 ) ) ;
#6297 = ORIENTED_EDGE ( 'NONE', *, *, #4577, .F. ) ;
#6298 = DIRECTION ( 'NONE',  ( 1.000000000000000000, 0.000000000000000000, 5.077734830647295768E-16 ) ) ;
#6299 = DIRECTION ( 'NONE',  ( -0.9396926207859097602, 0.3420201433256649381, -4.890320548438455808E-16 ) ) ;
#6300 = ORIENTED_EDGE ( 'NONE', *, *, #16115, .T. ) ;
#6301 = CONICAL_SURFACE ( 'NONE', #9912, 4.025000000000000355, 0.7853981633975870569 ) ;
#6302 = DIRECTION ( 'NONE',  ( 1.156482317317869999E-16, 0.000000000000000000, 1.000000000000000000 ) ) ;
#6303 = CARTESIAN_POINT ( 'NONE',  ( -68.99615306438117557, 2.010011688130281193, -15.00000000000001421 ) ) ;
#6304 = CIRCLE ( 'NONE', #6612, 4.599999999999992539 ) ;
#6305 = AXIS2_PLACEMENT_3D ( 'NONE', #14681, #6535, #3542 ) ;
#6306 = ORIENTED_EDGE ( 'NONE', *, *, #11684, .T. ) ;
#6307 = EDGE_LOOP ( 'NONE', ( #10343, #15749, #6797, #17422 ) ) ;
#6308 = ORIENTED_EDGE ( 'NONE', *, *, #3732, .F. ) ;
#6309 = CARTESIAN_POINT ( 'NONE',  ( -57.08002265617300708, 84.22855780814606419, -167.1454815528550739 ) ) ;
#6310 = CARTESIAN_POINT ( 'NONE',  ( -70.71978124295708312, -91.08423613455721579, 28.18308811886538479 ) ) ;
#6311 = AXIS2_PLACEMENT_3D ( 'NONE', #18502, #2965, #10080 ) ;
#6312 = VERTEX_POINT ( 'NONE', #10003 ) ;
#6313 = CARTESIAN_POINT ( 'NONE',  ( -54.80923614058017534, 94.79374675277698259, -167.1454815528550739 ) ) ;
#6314 = PLANE ( 'NONE',  #12053 ) ;
#6315 = DIRECTION ( 'NONE',  ( 1.000000000000000000, 0.000000000000000000, 0.000000000000000000 ) ) ;
#6316 = ORIENTED_EDGE ( 'NONE', *, *, #4260, .F. ) ;
#6317 = CYLINDRICAL_SURFACE ( 'NONE', #10470, 4.599999999999992539 ) ;
#6318 = AXIS2_PLACEMENT_3D ( 'NONE', #5109, #15216, #2398 ) ;
#6319 = AXIS2_PLACEMENT_3D ( 'NONE', #11247, #15142, #15237 ) ;
#6320 = FACE_OUTER_BOUND ( 'NONE', #4945, .T. ) ;
#6321 = CARTESIAN_POINT ( 'NONE',  ( -46.38449965345759551, 85.77305660501679085, -15.00000000000001421 ) ) ;
#6322 = DIRECTION ( 'NONE',  ( -1.000000000000000000, 0.000000000000000000, 0.000000000000000000 ) ) ;
#6323 = CARTESIAN_POINT ( 'NONE',  ( -17.00234300178814451, 45.78782387526246112, 30.07809993627739331 ) ) ;
#6324 = ORIENTED_EDGE ( 'NONE', *, *, #10308, .F. ) ;
#6325 = CARTESIAN_POINT ( 'NONE',  ( -57.08002265617300708, 84.22855780814606419, -47.49999999999999289 ) ) ;
#6326 = CARTESIAN_POINT ( 'NONE',  ( -57.08002265617300708, 84.22855780814606419, 35.00000000000000000 ) ) ;
#6327 = EDGE_LOOP ( 'NONE', ( #9231, #14767, #4625 ) ) ;
#6328 = CIRCLE ( 'NONE', #13811, 4.599999999999999645 ) ;
#6329 = LINE ( 'NONE', #2131, #9881 ) ;
#6330 =( NAMED_UNIT ( * ) PLANE_ANGLE_UNIT ( ) SI_UNIT ( $, .RADIAN. ) );
#6331 = ORIENTED_EDGE ( 'NONE', *, *, #7773, .F. ) ;
#6332 = ORIENTED_EDGE ( 'NONE', *, *, #12082, .F. ) ;
#6333 = AXIS2_PLACEMENT_3D ( 'NONE', #16741, #1238, #10032 ) ;
#6334 = VECTOR ( 'NONE', #2669, 1000.000000000000000 ) ;
#6335 = FACE_OUTER_BOUND ( 'NONE', #5039, .T. ) ;
#6336 = ORIENTED_EDGE ( 'NONE', *, *, #7229, .T. ) ;
#6337 = CARTESIAN_POINT ( 'NONE',  ( -68.99615306438074924, 120.7756765316626542, -167.1454815528550739 ) ) ;
#6338 = CARTESIAN_POINT ( 'NONE',  ( -71.24615306438114715, 10.00100075456375492, -167.1454815528550739 ) ) ;
#6339 = DIRECTION ( 'NONE',  ( 1.156482317317869999E-16, 0.000000000000000000, 1.000000000000000000 ) ) ;
#6340 = AXIS2_PLACEMENT_3D ( 'NONE', #9551, #5335, #1144 ) ;
#6341 = DIRECTION ( 'NONE',  ( 1.000000000000000000, 0.000000000000000000, 0.000000000000000000 ) ) ;
#6342 = LINE ( 'NONE', #16075, #17191 ) ;
#6343 = PLANE ( 'NONE',  #12934 ) ;
#6344 = ORIENTED_EDGE ( 'NONE', *, *, #16092, .T. ) ;
#6345 = CARTESIAN_POINT ( 'NONE',  ( 0.000000000000000000, 0.000000000000000000, 57.00000000000000000 ) ) ;
#6346 = VECTOR ( 'NONE', #11534, 1000.000000000000000 ) ;
#6347 = VECTOR ( 'NONE', #13665, 1000.000000000000000 ) ;
#6348 = VECTOR ( 'NONE', #6912, 1000.000000000000000 ) ;
#6349 = DIRECTION ( 'NONE',  ( -1.000000000000000000, 0.000000000000000000, -5.204170427930409450E-16 ) ) ;
#6350 = ORIENTED_EDGE ( 'NONE', *, *, #5351, .T. ) ;
#6351 = CARTESIAN_POINT ( 'NONE',  ( -31.40585197410439378, -91.08930925317537231, -10.39386867823087002 ) ) ;
#6352 = CARTESIAN_POINT ( 'NONE',  ( -57.08002265617300708, 84.22855780814606419, -47.50000000000000000 ) ) ;
#6353 = ORIENTED_EDGE ( 'NONE', *, *, #934, .T. ) ;
#6354 = ORIENTED_EDGE ( 'NONE', *, *, #1285, .T. ) ;
#6355 = ADVANCED_FACE ( 'NONE', ( #7100 ), #16917, .T. ) ;
#6356 =( GEOMETRIC_REPRESENTATION_CONTEXT ( 3 ) GLOBAL_UNCERTAINTY_ASSIGNED_CONTEXT ( ( #18068 ) ) GLOBAL_UNIT_ASSIGNED_CONTEXT ( ( #13261, #16874, #13895 ) ) REPRESENTATION_CONTEXT ( 'NONE', 'WORKASPACE' ) );
#6357 = VECTOR ( 'NONE', #2955, 1000.000000000000000 ) ;
#6358 = AXIS2_PLACEMENT_3D ( 'NONE', #6775, #15176, #12401 ) ;
#6359 = CARTESIAN_POINT ( 'NONE',  ( -68.99615306438109030, 17.10311908166270456, -167.1454815528550739 ) ) ;
#6360 = DIRECTION ( 'NONE',  ( 1.000000000000000000, 0.000000000000000000, -0.000000000000000000 ) ) ;
#6361 = CARTESIAN_POINT ( 'NONE',  ( -70.71978124295668522, -111.0842361345572158, -28.18308811886538479 ) ) ;
#6362 = CARTESIAN_POINT ( 'NONE',  ( -212.2032458117903104, 84.22855780814606419, 62.50000000000001421 ) ) ;
#6363 = EDGE_LOOP ( 'NONE', ( #986, #16904, #13409, #806, #4111, #1458 ) ) ;
#6364 = LINE ( 'NONE', #5056, #17308 ) ;
#6365 = DIRECTION ( 'NONE',  ( 0.000000000000000000, 0.000000000000000000, 1.000000000000000000 ) ) ;
#6366 = ORIENTED_EDGE ( 'NONE', *, *, #3796, .F. ) ;
#6367 = FACE_OUTER_BOUND ( 'NONE', #15451, .T. ) ;
#6368 = CARTESIAN_POINT ( 'NONE',  ( -107.5926225674731853, 102.8748711238780373, 20.00000000000000355 ) ) ;
#6369 = FACE_OUTER_BOUND ( 'NONE', #7235, .T. ) ;
#6370 = CARTESIAN_POINT ( 'NONE',  ( 0.05458999538779253646, -1.264741368073575511, -6.500000000000063949 ) ) ;
#6371 = EDGE_LOOP ( 'NONE', ( #5477, #12108, #2282, #2735 ) ) ;
#6372 = EDGE_CURVE ( 'NONE', #10372, #4288, #18334, .T. ) ;
#6373 = DIRECTION ( 'NONE',  ( 1.000000000000000000, 0.000000000000000000, 0.000000000000000000 ) ) ;
#6374 = VERTEX_POINT ( 'NONE', #14299 ) ;
#6375 = EDGE_CURVE ( 'NONE', #11376, #18033, #5504, .T. ) ;
#6376 = VECTOR ( 'NONE', #18219, 1000.000000000000000 ) ;
#6377 = CARTESIAN_POINT ( 'NONE',  ( 56.85086857400936822, 84.22855780814606419, 70.00000000000001421 ) ) ;
#6379 = EDGE_LOOP ( 'NONE', ( #15275, #3623, #4089, #5442 ) ) ;
#6378 = AXIS2_PLACEMENT_3D ( 'NONE', #4418, #1533, #11365 ) ;
#6380 = PRODUCT ( 'High-Ratio Toggle Operating Handle', 'High-Ratio Toggle Operating Handle', '', ( #8278 ) ) ;
#6381 = ORIENTED_EDGE ( 'NONE', *, *, #13161, .T. ) ;
#6382 = ADVANCED_FACE ( 'NONE', ( #12809 ), #15786, .T. ) ;
#6383 = PRESENTATION_LAYER_ASSIGNMENT (  '', '', ( #6710 ) ) ;
#6384 = EDGE_CURVE ( 'NONE', #7201, #13332, #14121, .T. ) ;
#6385 = CARTESIAN_POINT ( 'NONE',  ( -48.13268001719898592, 75.49957964911752129, -167.1454815528550739 ) ) ;
#6386 = DIRECTION ( 'NONE',  ( 0.000000000000000000, 0.000000000000000000, 1.000000000000000000 ) ) ;
#6387 = VECTOR ( 'NONE', #912, 1000.000000000000000 ) ;
#6388 = VERTEX_POINT ( 'NONE', #14222 ) ;
#6389 = AXIS2_PLACEMENT_3D ( 'NONE', #13334, #3049, #14469 ) ;
#6390 = CARTESIAN_POINT ( 'NONE',  ( -83.12361985383351737, 84.22855780814606419, -35.00000000000000711 ) ) ;
#6391 = PLANE ( 'NONE',  #7028 ) ;
#6392 = ORIENTED_EDGE ( 'NONE', *, *, #4904, .T. ) ;
#6393 = DIRECTION ( 'NONE',  ( -0.000000000000000000, -1.000000000000000000, -0.000000000000000000 ) ) ;
#6394 = EDGE_CURVE ( 'NONE', #1115, #13953, #1398, .T. ) ;
#6395 = ORIENTED_EDGE ( 'NONE', *, *, #10334, .T. ) ;
#6396 = EDGE_CURVE ( 'NONE', #15625, #15720, #15249, .T. ) ;
#6397 = CYLINDRICAL_SURFACE ( 'NONE', #9927, 26.04359719766049253 ) ;
#6398 = LINE ( 'NONE', #15189, #1564 ) ;
#6399 = ORIENTED_EDGE ( 'NONE', *, *, #2892, .T. ) ;
#6400 = EDGE_CURVE ( 'NONE', #12790, #5784, #983, .T. ) ;
#6401 = VECTOR ( 'NONE', #2256, 1000.000000000000000 ) ;
#6402 = B_SPLINE_CURVE_WITH_KNOTS ( 'NONE', 3,
 ( #14695, #7598, #491, #4966, #16371, #5053, #10771, #13218, #16465, #397 ),
 .UNSPECIFIED., .F., .F.,
 ( 4, 2, 2, 2, 4 ),
 ( 0.006898123196567208619, 0.01082895749156352269, 0.01279437463906168276, 0.01475979178655984284, 0.02262146037655243455 ),
 .UNSPECIFIED. ) ;
#6403 = LINE ( 'NONE', #713, #10015 ) ;
#6404 = EDGE_CURVE ( 'NONE', #10454, #13894, #9573, .T. ) ;
#6405 = AXIS2_PLACEMENT_3D ( 'NONE', #8508, #5676, #7097 ) ;
#6406 = CARTESIAN_POINT ( 'NONE',  ( -94.45685920050698314, -47.21335801510345220, 15.00000000000006928 ) ) ;
#6407 = VECTOR ( 'NONE', #11877, 1000.000000000000000 ) ;
#6408 = ORIENTED_EDGE ( 'NONE', *, *, #15877, .F. ) ;
#6409 = VECTOR ( 'NONE', #15437, 1000.000000000000000 ) ;
#6410 = ADVANCED_FACE ( 'NONE', ( #10992 ), #18194, .T. ) ;
#6411 = EDGE_CURVE ( 'NONE', #1616, #5307, #12592, .T. ) ;
#6412 = EDGE_CURVE ( 'NONE', #2362, #11975, #15867, .T. ) ;
#6413 = EDGE_LOOP ( 'NONE', ( #8226, #9205, #6208, #11206 ) ) ;
#6414 = CARTESIAN_POINT ( 'NONE',  ( -47.13906347517657025, 79.99098546104539764, 15.00000000000009592 ) ) ;
#6415 = CARTESIAN_POINT ( 'NONE',  ( -57.56709772515574031, 94.46597735006069740, -167.1454815528550739 ) ) ;
#6416 = EDGE_LOOP ( 'NONE', ( #11296, #3575, #10565, #14583 ) ) ;
#6417 = DIRECTION ( 'NONE',  ( 0.000000000000000000, 1.000000000000000000, -0.000000000000000000 ) ) ;
#6418 = CARTESIAN_POINT ( 'NONE',  ( 4.873448657480574653, -11.10503745953439569, 53.31400367155413278 ) ) ;
#6419 = CARTESIAN_POINT ( 'NONE',  ( -71.24615306438086293, 93.93513156522925556, -167.1454815528550739 ) ) ;
#6420 = ORIENTED_EDGE ( 'NONE', *, *, #15221, .T. ) ;
#6421 = VECTOR ( 'NONE', #2541, 1000.000000000000000 ) ;
#6422 = DIRECTION ( 'NONE',  ( -1.000000000000000000, 0.000000000000000000, 0.000000000000000000 ) ) ;
#6423 = PRESENTATION_LAYER_ASSIGNMENT (  '', '', ( #16892 ) ) ;
#6424 = PLANE ( 'NONE',  #4063 ) ;
#6425 = DIRECTION ( 'NONE',  ( 0.3420201433256407353, -0.9396926207859186420, 0.000000000000000000 ) ) ;
#6426 = VECTOR ( 'NONE', #12436, 1000.000000000000000 ) ;
#6427 = DIRECTION ( 'NONE',  ( 1.000000000000000000, 0.000000000000000000, 0.000000000000000000 ) ) ;
#6428 = VERTEX_POINT ( 'NONE', #10800 ) ;
#6429 = EDGE_CURVE ( 'NONE', #16609, #16158, #14955, .T. ) ;
#6430 = DIRECTION ( 'NONE',  ( -0.9396926207859145341, 0.3420201433256519485, -4.890320548438481446E-16 ) ) ;
#6431 = DIRECTION ( 'NONE',  ( -1.000000000000000000, -0.000000000000000000, -0.000000000000000000 ) ) ;
#6432 = EDGE_CURVE ( 'NONE', #2011, #70, #5464, .T. ) ;
#6433 = ORIENTED_EDGE ( 'NONE', *, *, #6289, .F. ) ;
#6434 = PLANE ( 'NONE',  #17915 ) ;
#6435 = CARTESIAN_POINT ( 'NONE',  ( -37.14175463882769890, 77.49513323845337709, 65.84001190467381548 ) ) ;
#6436 = ORIENTED_EDGE ( 'NONE', *, *, #3008, .F. ) ;
#6437 = ORIENTED_EDGE ( 'NONE', *, *, #4689, .F. ) ;
#6438 = CIRCLE ( 'NONE', #12128, 5.000000000000004441 ) ;
#6439 = CARTESIAN_POINT ( 'NONE',  ( -93.73308511844572877, 147.7866419848965052, -15.00000000000001421 ) ) ;
#6440 = ORIENTED_EDGE ( 'NONE', *, *, #18454, .T. ) ;
#6441 = B_SPLINE_CURVE_WITH_KNOTS ( 'NONE', 3,
 ( #13730, #18032, #13827, #15219, #9614, #11025, #3905, #10653, #2405, #1116, #15316, #1016, #12443, #18135, #16709, #16338, #8218, #6810, #3524, #9239 ),
 .UNSPECIFIED., .F., .F.,
 ( 4, 2, 2, 2, 2, 2, 2, 2, 2, 4 ),
 ( -1.439925654488133212E-05, 0.0006244272253376713638, 0.001263253707220224212, 0.002540906670985296299, 0.003818559634750368168, 0.005096212598515426594, 0.006373865562280486320, 0.007651518526045546914, 0.008929171489810606641, 0.01020682445357566810 ),
 .UNSPECIFIED. ) ;
#6442 = LINE ( 'NONE', #12162, #6097 ) ;
#6443 = CARTESIAN_POINT ( 'NONE',  ( -54.75080917176597950, 94.79374675277695417, -15.00000000000001421 ) ) ;
#6444 = CARTESIAN_POINT ( 'NONE',  ( -71.24615306438086293, 93.93513156522925556, 15.00000000000006928 ) ) ;
#6445 = DIRECTION ( 'NONE',  ( 0.000000000000000000, 1.000000000000000000, -1.224646799147353207E-16 ) ) ;
#6446 = LINE ( 'NONE', #10383, #2856 ) ;
#6447 = CARTESIAN_POINT ( 'NONE',  ( -71.24615306438079188, 107.3903729045637192, -15.00000000000001421 ) ) ;
#6448 = ORIENTED_EDGE ( 'NONE', *, *, #2895, .T. ) ;
#6449 = CARTESIAN_POINT ( 'NONE',  ( -73.36356571042369978, 59.78633783786654021, -22.83555841014880272 ) ) ;
#6450 = DIRECTION ( 'NONE',  ( 0.000000000000000000, 0.000000000000000000, 1.000000000000000000 ) ) ;
#6451 = ORIENTED_EDGE ( 'NONE', *, *, #17272, .F. ) ;
#6452 = CARTESIAN_POINT ( 'NONE',  ( -71.24615306438089135, 84.51035361522924916, -15.00000000000001421 ) ) ;
#6453 = LINE ( 'NONE', #13384, #2658 ) ;
#6454 = ORIENTED_EDGE ( 'NONE', *, *, #1081, .T. ) ;
#6455 = VERTEX_POINT ( 'NONE', #11187 ) ;
#6456 = CARTESIAN_POINT ( 'NONE',  ( 124.5381772159375942, -46.83756720124470263, 115.7605492041889619 ) ) ;
#6457 = DIRECTION ( 'NONE',  ( 1.156482317317869999E-16, 0.000000000000000000, 1.000000000000000000 ) ) ;
#6458 = DIRECTION ( 'NONE',  ( 0.000000000000000000, 1.000000000000000000, -0.000000000000000000 ) ) ;
#6459 = EDGE_CURVE ( 'NONE', #1208, #8420, #4077, .T. ) ;
#6460 = DIRECTION ( 'NONE',  ( 0.000000000000000000, 0.000000000000000000, -1.000000000000000000 ) ) ;
#6461 = VERTEX_POINT ( 'NONE', #1174 ) ;
#6462 = CARTESIAN_POINT ( 'NONE',  ( 3.930119462001817841E-14, -91.08423613455721579, -5.654315315325195712 ) ) ;
#6463 = CARTESIAN_POINT ( 'NONE',  ( -68.99615306438072082, 130.8153103381302742, -167.1454815528550739 ) ) ;
#6464 = ORIENTED_EDGE ( 'NONE', *, *, #12027, .T. ) ;
#6465 = CARTESIAN_POINT ( 'NONE',  ( -71.24615306438114715, 16.28418605456380419, -15.00000000000001421 ) ) ;
#6466 = FACE_OUTER_BOUND ( 'NONE', #17781, .T. ) ;
#6467 = CARTESIAN_POINT ( 'NONE',  ( -76.76096363794077604, 91.67867170800820986, 61.50632582155040495 ) ) ;
#6468 = CARTESIAN_POINT ( 'NONE',  ( 5.303146227817084385E-14, -0.6346842323190391433, -6.500000000000061284 ) ) ;
#6469 = EDGE_LOOP ( 'NONE', ( #14425, #16674, #4695, #15512 ) ) ;
#6470 = CARTESIAN_POINT ( 'NONE',  ( -57.08002265617300708, 84.22855780814606419, 15.00000000000006928 ) ) ;
#6471 = ORIENTED_EDGE ( 'NONE', *, *, #786, .T. ) ;
#6472 = CARTESIAN_POINT ( 'NONE',  ( -71.24615306438091977, 72.83285375456371469, -15.00000000000001421 ) ) ;
#6473 = ORIENTED_EDGE ( 'NONE', *, *, #5346, .T. ) ;
#6474 = ORIENTED_EDGE ( 'NONE', *, *, #18277, .F. ) ;
#6475 = PLANE ( 'NONE',  #11198 ) ;
#6476 = FACE_OUTER_BOUND ( 'NONE', #10481, .T. ) ;
#6477 = ORIENTED_EDGE ( 'NONE', *, *, #9596, .F. ) ;
#6478 = EDGE_CURVE ( 'NONE', #10978, #12641, #13796, .T. ) ;
#6479 = LINE ( 'NONE', #12117, #17946 ) ;
#6480 = DIRECTION ( 'NONE',  ( 0.000000000000000000, 1.000000000000000000, 0.000000000000000000 ) ) ;
#6481 = ORIENTED_EDGE ( 'NONE', *, *, #11095, .F. ) ;
#6482 = CARTESIAN_POINT ( 'NONE',  ( -68.99615306438106188, 30.28434553813027108, -167.1454815528550739 ) ) ;
#6483 = CARTESIAN_POINT ( 'NONE',  ( 0.000000000000000000, 7.505553499465141165, -1.387778780781445676E-14 ) ) ;
#6484 = ORIENTED_EDGE ( 'NONE', *, *, #18207, .T. ) ;
#6485 = DIRECTION ( 'NONE',  ( 0.9396926207859097602, 0.3420201433256649381, 4.890320548438455808E-16 ) ) ;
#6486 = CARTESIAN_POINT ( 'NONE',  ( -67.25621515281476093, 107.4062629095552808, 25.00000000000000355 ) ) ;
#6487 = VERTEX_POINT ( 'NONE', #6685 ) ;
#6488 = EDGE_CURVE ( 'NONE', #4573, #5742, #9484, .T. ) ;
#6489 = MANIFOLD_SOLID_BREP ( 'Fillet6', #17729 ) ;
#6490 = DIRECTION ( 'NONE',  ( -1.000000000000000000, 0.000000000000000000, 0.000000000000000000 ) ) ;
#6491 = LINE ( 'NONE', #3593, #11970 ) ;
#6492 = EDGE_LOOP ( 'NONE', ( #9883, #1281, #7302, #438 ) ) ;
#6493 = ADVANCED_FACE ( 'NONE', ( #15285 ), #16774, .F. ) ;
#6494 = EDGE_LOOP ( 'NONE', ( #3430, #338, #10917, #14213 ) ) ;
#6495 = EDGE_CURVE ( 'NONE', #12009, #2102, #9779, .T. ) ;
#6496 = CARTESIAN_POINT ( 'NONE',  ( -97.59262256747318531, 0.3328663868096687350, -25.00000000000000000 ) ) ;
#6497 = CARTESIAN_POINT ( 'NONE',  ( -68.99615306438097662, 57.94382353166266597, -167.1454815528550739 ) ) ;
#6498 = EDGE_CURVE ( 'NONE', #5337, #11425, #41, .T. ) ;
#6499 = VERTEX_POINT ( 'NONE', #11284 ) ;
#6500 = DIRECTION ( 'NONE',  ( 1.000000000000000000, 0.000000000000000000, 0.000000000000000000 ) ) ;
#6501 =( LENGTH_UNIT ( ) NAMED_UNIT ( * ) SI_UNIT ( .MILLI., .METRE. ) );
#6502 = CARTESIAN_POINT ( 'NONE',  ( -61.80899203128051056, 95.79950628479635100, -167.1454815528550739 ) ) ;
#6503 = DIRECTION ( 'NONE',  ( 0.000000000000000000, 0.000000000000000000, 1.000000000000000000 ) ) ;
#6504 = DIRECTION ( 'NONE',  ( 1.000000000000000000, 0.000000000000000000, 0.000000000000000000 ) ) ;
#6505 = ORIENTED_EDGE ( 'NONE', *, *, #2283, .F. ) ;
#6506 = CARTESIAN_POINT ( 'NONE',  ( -71.24615306438076345, 131.6342433652292243, 15.00000000000006928 ) ) ;
#6507 = DIRECTION ( 'NONE',  ( 1.000000000000000000, 2.062304371594500494E-16, -2.775557561562890858E-16 ) ) ;
#6508 = FACE_OUTER_BOUND ( 'NONE', #15516, .T. ) ;
#6509 = AXIS2_PLACEMENT_3D ( 'NONE', #7060, #12772, #15659 ) ;
#6510 = DIRECTION ( 'NONE',  ( -0.000000000000000000, -0.000000000000000000, 1.000000000000000000 ) ) ;
#6511 = ORIENTED_EDGE ( 'NONE', *, *, #12951, .F. ) ;
#6512 = EDGE_CURVE ( 'NONE', #961, #10265, #15839, .T. ) ;
#6513 = ADVANCED_FACE ( 'NONE', ( #3030 ), #6286, .T. ) ;
#6514 = EDGE_CURVE ( 'NONE', #12457, #10530, #1245, .T. ) ;
#6515 = CYLINDRICAL_SURFACE ( 'NONE', #14490, 10.24900000000000766 ) ;
#6516 = DIRECTION ( 'NONE',  ( 0.3420201433256444545, 0.9396926207859171987, -0.000000000000000000 ) ) ;
#6517 = ORIENTED_EDGE ( 'NONE', *, *, #6167, .T. ) ;
#6518 = EDGE_CURVE ( 'NONE', #1656, #15261, #17060, .T. ) ;
#6519 = CARTESIAN_POINT ( 'NONE',  ( -68.99615306438094819, 64.22700883166265839, 15.00000000000006928 ) ) ;
#6520 = CARTESIAN_POINT ( 'NONE',  ( -37.27023256319369438, 77.12848153769259341, 60.07106347578592676 ) ) ;
#6521 = VERTEX_POINT ( 'NONE', #8745 ) ;
#6522 = ORIENTED_EDGE ( 'NONE', *, *, #11119, .F. ) ;
#6523 = ADVANCED_FACE ( 'NONE', ( #5743 ), #8843, .T. ) ;
#6524 = AXIS2_PLACEMENT_3D ( 'NONE', #11602, #9830, #718 ) ;
#6525 = DIRECTION ( 'NONE',  ( 0.000000000000000000, 0.000000000000000000, 1.000000000000000000 ) ) ;
#6526 = EDGE_LOOP ( 'NONE', ( #133, #16452, #9469, #2745 ) ) ;
#6527 = EDGE_CURVE ( 'NONE', #616, #3601, #8566, .T. ) ;
#6528 = CARTESIAN_POINT ( 'NONE',  ( -57.08002265617300708, 84.22855780814606419, -15.00000000000001421 ) ) ;
#6529 = LINE ( 'NONE', #12352, #7268 ) ;
#6530 = EDGE_CURVE ( 'NONE', #455, #7544, #5834, .T. ) ;
#6531 = DIRECTION ( 'NONE',  ( 0.000000000000000000, -5.551115123125748189E-17, -1.000000000000000000 ) ) ;
#6532 = CYLINDRICAL_SURFACE ( 'NONE', #2387, 10.24900000000000055 ) ;
#6533 = LINE ( 'NONE', #12543, #12104 ) ;
#6534 = DIRECTION ( 'NONE',  ( 1.000000000000000000, 0.000000000000000000, 0.000000000000000000 ) ) ;
#6535 = DIRECTION ( 'NONE',  ( 0.000000000000000000, 0.000000000000000000, 1.000000000000000000 ) ) ;
#6536 = ORIENTED_EDGE ( 'NONE', *, *, #10666, .T. ) ;
#6537 = EDGE_CURVE ( 'NONE', #11339, #14706, #12784, .T. ) ;
#6538 = DIRECTION ( 'NONE',  ( -1.000000000000000000, 0.000000000000000000, 0.000000000000000000 ) ) ;
#6539 = FACE_BOUND ( 'NONE', #11372, .T. ) ;
#6540 = VECTOR ( 'NONE', #1292, 1000.000000000000000 ) ;
#6541 = ORIENTED_EDGE ( 'NONE', *, *, #14261, .F. ) ;
#6542 = CARTESIAN_POINT ( 'NONE',  ( -67.59262256747315689, 129.5689604715732912, -15.00000000000001066 ) ) ;
#6543 = CARTESIAN_POINT ( 'NONE',  ( -194.4437806548868934, -151.5628872026273086, 18.23991632971911869 ) ) ;
#6544 = ORIENTED_EDGE ( 'NONE', *, *, #4682, .T. ) ;
#6545 = EDGE_LOOP ( 'NONE', ( #654, #10782, #3902, #15143 ) ) ;
#6546 = ORIENTED_EDGE ( 'NONE', *, *, #17152, .F. ) ;
#6547 = CARTESIAN_POINT ( 'NONE',  ( -54.80923614058017534, 94.79374675277698259, 15.00000000000006928 ) ) ;
#6548 = DIRECTION ( 'NONE',  ( 1.156482317317869999E-16, 0.000000000000000000, 1.000000000000000000 ) ) ;
#6549 = VECTOR ( 'NONE', #15762, 1000.000000000000000 ) ;
#6550 = CARTESIAN_POINT ( 'NONE',  ( -68.99615306438106188, 35.95267498166268894, 15.00000000000006928 ) ) ;
#6551 = DIRECTION ( 'NONE',  ( -1.000000000000000000, 0.000000000000000000, 0.000000000000000000 ) ) ;
#6552 = DIRECTION ( 'NONE',  ( 0.000000000000000000, 0.000000000000000000, 1.000000000000000000 ) ) ;
#6553 = CIRCLE ( 'NONE', #16403, 10.24900000000000055 ) ;
#6554 = DIRECTION ( 'NONE',  ( 0.000000000000000000, 0.000000000000000000, 1.000000000000000000 ) ) ;
#6555 = ORIENTED_EDGE ( 'NONE', *, *, #5433, .F. ) ;
#6556 = ADVANCED_BREP_SHAPE_REPRESENTATION ( '', ( #6144, #16217 ), #11478 ) ;
#6557 = CARTESIAN_POINT ( 'NONE',  ( 0.000000000000000000, 0.000000000000000000, 0.000000000000000000 ) ) ;
#6558 = CARTESIAN_POINT ( 'NONE',  ( -60.71399380653853228, 72.26844686893187486, 15.00000000000006928 ) ) ;
#6560 = EDGE_LOOP ( 'NONE', ( #14615, #17110, #3075, #1028 ) ) ;
#6559 = DIRECTION ( 'NONE',  ( -0.000000000000000000, -1.000000000000000000, -0.000000000000000000 ) ) ;
#6561 = DIRECTION ( 'NONE',  ( 0.000000000000000000, 0.000000000000000000, 1.000000000000000000 ) ) ;
#6562 = VERTEX_POINT ( 'NONE', #7341 ) ;
#6563 = DIRECTION ( 'NONE',  ( 0.000000000000000000, 0.000000000000000000, 1.000000000000000000 ) ) ;
#6564 = ORIENTED_EDGE ( 'NONE', *, *, #539, .F. ) ;
#6565 = LINE ( 'NONE', #6853, #12816 ) ;
#6566 = ORIENTED_EDGE ( 'NONE', *, *, #16938, .T. ) ;
#6567 = VECTOR ( 'NONE', #13973, 1000.000000000000000 ) ;
#6568 = PRODUCT_DEFINITION ( 'UNKNOWN', '', #4598, #13581 ) ;
#6569 = AXIS2_PLACEMENT_3D ( 'NONE', #4490, #17221, #1970 ) ;
#6570 = AXIS2_PLACEMENT_3D ( 'NONE', #6831, #2721, #2824 ) ;
#6571 = VERTEX_POINT ( 'NONE', #5909 ) ;
#6572 = DIRECTION ( 'NONE',  ( 1.000000000000000000, 0.000000000000000000, 0.000000000000000000 ) ) ;
#6573 = FACE_OUTER_BOUND ( 'NONE', #17607, .T. ) ;
#6574 = ORIENTED_EDGE ( 'NONE', *, *, #5471, .F. ) ;
#6575 = PRODUCT_CONTEXT ( 'NONE', #13873, 'mechanical' ) ;
#6576 = VECTOR ( 'NONE', #8432, 1000.000000000000000 ) ;
#6577 = CYLINDRICAL_SURFACE ( 'NONE', #15271, 5.654315315325680658 ) ;
#6578 = VECTOR ( 'NONE', #537, 1000.000000000000000 ) ;
#6579 = DIRECTION ( 'NONE',  ( 1.000000000000000000, -0.000000000000000000, -0.000000000000000000 ) ) ;
#6580 = ORIENTED_EDGE ( 'NONE', *, *, #18180, .T. ) ;
#6581 = DIRECTION ( 'NONE',  ( 0.000000000000000000, 0.000000000000000000, 1.000000000000000000 ) ) ;
#6582 = DIRECTION ( 'NONE',  ( -0.000000000000000000, -0.000000000000000000, -1.000000000000000000 ) ) ;
#6583 = VECTOR ( 'NONE', #18025, 1000.000000000000000 ) ;
#6584 = ORIENTED_EDGE ( 'NONE', *, *, #242, .F. ) ;
#6585 = CIRCLE ( 'NONE', #8990, 7.168074330098680669 ) ;
#6586 = CARTESIAN_POINT ( 'NONE',  ( -76.06755393367096474, 106.6341280094858490, -25.60850497571804496 ) ) ;
#6587 = LINE ( 'NONE', #13620, #8435 ) ;
#6588 = ORIENTED_EDGE ( 'NONE', *, *, #16115, .F. ) ;
#6589 = CARTESIAN_POINT ( 'NONE',  ( -68.99615306438072082, 127.0588618316627105, -15.00000000000001421 ) ) ;
#6590 = VECTOR ( 'NONE', #2367, 1000.000000000000000 ) ;
#6591 = CARTESIAN_POINT ( 'NONE',  ( -81.24478565583270040, -91.08423613455721579, -39.14322682088991456 ) ) ;
#6592 = EDGE_LOOP ( 'NONE', ( #16858, #7700, #1919, #1706 ) ) ;
#6593 = AXIS2_PLACEMENT_3D ( 'NONE', #14084, #2583, #12306 ) ;
#6594 = AXIS2_PLACEMENT_3D ( 'NONE', #13076, #4627, #13333 ) ;
#6595 = ORIENTED_EDGE ( 'NONE', *, *, #4566, .F. ) ;
#6596 = DIRECTION ( 'NONE',  ( -2.062304371594500494E-16, 1.000000000000000000, -0.000000000000000000 ) ) ;
#6597 = CARTESIAN_POINT ( 'NONE',  ( -48.74405704658271077, 91.10542963993684396, -15.00000000000001421 ) ) ;
#6598 = ORIENTED_EDGE ( 'NONE', *, *, #8272, .T. ) ;
#6599 = EDGE_CURVE ( 'NONE', #10149, #9739, #627, .T. ) ;
#6600 = CARTESIAN_POINT ( 'NONE',  ( -67.20241558018224737, 85.83453492254335515, -167.1454815528550739 ) ) ;
#6601 = CARTESIAN_POINT ( 'NONE',  ( -76.76083043436963749, 76.77809071147591169, 61.50853494822962375 ) ) ;
#6602 = DIRECTION ( 'NONE',  ( 1.000000000000000000, 0.000000000000000000, 0.000000000000000000 ) ) ;
#6603 = LINE ( 'NONE', #6419, #9686 ) ;
#6604 = ORIENTED_EDGE ( 'NONE', *, *, #7953, .T. ) ;
#6605 = VECTOR ( 'NONE', #17225, 1000.000000000000000 ) ;
#6606 = CARTESIAN_POINT ( 'NONE',  ( -65.06546592763146464, -111.0842361345572158, 45.05044770573184110 ) ) ;
#6607 = FACE_OUTER_BOUND ( 'NONE', #15814, .T. ) ;
#6608 = CARTESIAN_POINT ( 'NONE',  ( -71.24615306438083451, 97.96559495456375544, -15.00000000000001421 ) ) ;
#6609 = FACE_OUTER_BOUND ( 'NONE', #6793, .T. ) ;
#6610 = LINE ( 'NONE', #15126, #7243 ) ;
#6611 = EDGE_LOOP ( 'NONE', ( #18113, #3340, #9771, #15323 ) ) ;
#6612 = AXIS2_PLACEMENT_3D ( 'NONE', #1856, #14498, #6135 ) ;
#6613 = VECTOR ( 'NONE', #15910, 1000.000000000000000 ) ;
#6614 = CARTESIAN_POINT ( 'NONE',  ( -71.24615306438103346, 40.52805651522925245, 15.00000000000006928 ) ) ;
#6615 = LINE ( 'NONE', #10730, #1233 ) ;
#6616 = EDGE_CURVE ( 'NONE', #9284, #2271, #6913, .T. ) ;
#6617 = ORIENTED_EDGE ( 'NONE', *, *, #1025, .F. ) ;
#6618 = FACE_OUTER_BOUND ( 'NONE', #14555, .T. ) ;
#6619 = CARTESIAN_POINT ( 'NONE',  ( -37.14248503629701048, 77.49305091727374872, 59.16519171840705127 ) ) ;
#6620 = ORIENTED_EDGE ( 'NONE', *, *, #5280, .T. ) ;
#6621 = ORIENTED_EDGE ( 'NONE', *, *, #10655, .F. ) ;
#6622 = VECTOR ( 'NONE', #12124, 1000.000000000000000 ) ;
#6623 = CARTESIAN_POINT ( 'NONE',  ( -92.59262256747321373, 106.8071537307723133, -25.00000000000000000 ) ) ;
#6624 = EDGE_CURVE ( 'NONE', #5917, #10712, #1449, .T. ) ;
#6625 = ORIENTED_EDGE ( 'NONE', *, *, #8889, .F. ) ;
#6626 = EDGE_CURVE ( 'NONE', #10960, #9281, #6970, .T. ) ;
#6627 = AXIS2_PLACEMENT_3D ( 'NONE', #2219, #12440, #6715 ) ;
#6628 = CIRCLE ( 'NONE', #14127, 12.58237727243326987 ) ;
#6629 = DIRECTION ( 'NONE',  ( -0.9396926207859084279, 0.3420201433256687684, -4.890320548438449892E-16 ) ) ;
#6630 = CARTESIAN_POINT ( 'NONE',  ( -62.81538793034061285, 92.72253132893551708, -167.1454815528550739 ) ) ;
#6631 = CARTESIAN_POINT ( 'NONE',  ( -66.20309715099607217, 56.86452048533069359, 24.99999999999999645 ) ) ;
#6632 = DIRECTION ( 'NONE',  ( 0.3420201433256686574, -0.9396926207859084279, 0.000000000000000000 ) ) ;
#6633 = DIRECTION ( 'NONE',  ( 0.000000000000000000, 0.000000000000000000, 1.000000000000000000 ) ) ;
#6634 = PLANE ( 'NONE',  #1645 ) ;
#6635 = CARTESIAN_POINT ( 'NONE',  ( -46.03642545851250389, 84.22855780814606419, -62.50000000000000000 ) ) ;
#6636 = ORIENTED_EDGE ( 'NONE', *, *, #7284, .F. ) ;
#6637 = EDGE_CURVE ( 'NONE', #162, #15245, #11555, .T. ) ;
#6638 = AXIS2_PLACEMENT_3D ( 'NONE', #15753, #11720, #15836 ) ;
#6639 = DIRECTION ( 'NONE',  ( -1.000000000000000000, 0.000000000000000000, 0.000000000000000000 ) ) ;
#6640 = LINE ( 'NONE', #1132, #1787 ) ;
#6641 = EDGE_CURVE ( 'NONE', #10712, #18436, #12869, .T. ) ;
#6642 = ORIENTED_EDGE ( 'NONE', *, *, #17478, .T. ) ;
#6643 = CIRCLE ( 'NONE', #10524, 2.168074330099287295 ) ;
#6644 = CARTESIAN_POINT ( 'NONE',  ( -25.73217265163131984, -95.23217577251028843, -5.709860606646929071 ) ) ;
#6645 = AXIS2_PLACEMENT_3D ( 'NONE', #2764, #17163, #2584 ) ;
#6646 = DIRECTION ( 'NONE',  ( 1.000000000000000000, 0.000000000000000000, 0.000000000000000000 ) ) ;
#6647 = ADVANCED_FACE ( 'NONE', ( #10056 ), #4161, .T. ) ;
#6648 = VERTEX_POINT ( 'NONE', #17067 ) ;
#6649 = EDGE_CURVE ( 'NONE', #11466, #12161, #3301, .T. ) ;
#6650 = VERTEX_POINT ( 'NONE', #9967 ) ;
#6651 = ORIENTED_EDGE ( 'NONE', *, *, #1042, .F. ) ;
#6652 = UNCERTAINTY_MEASURE_WITH_UNIT (LENGTH_MEASURE( 1.000000000000000082E-05 ), #6215, 'distance_accuracy_value', 'NONE');
#6653 = ADVANCED_FACE ( 'NONE', ( #10137 ), #6269, .T. ) ;
#6654 = VECTOR ( 'NONE', #11159, 1000.000000000000000 ) ;
#6655 = FACE_OUTER_BOUND ( 'NONE', #11314, .T. ) ;
#6656 = DIRECTION ( 'NONE',  ( 0.000000000000000000, 1.000000000000000000, 0.000000000000000000 ) ) ;
#6657 = DIRECTION ( 'NONE',  ( -1.000000000000000000, -0.000000000000000000, -0.000000000000000000 ) ) ;
#6658 = DIRECTION ( 'NONE',  ( 0.000000000000000000, 0.000000000000000000, 1.000000000000000000 ) ) ;
#6659 = AXIS2_PLACEMENT_3D ( 'NONE', #6939, #13868, #12470 ) ;
#6660 = CIRCLE ( 'NONE', #17122, 4.000000000000003553 ) ;
#6661 = LINE ( 'NONE', #9657, #9612 ) ;
#6662 = ORIENTED_EDGE ( 'NONE', *, *, #10663, .T. ) ;
#6663 = LINE ( 'NONE', #13593, #4523 ) ;
#6664 = CARTESIAN_POINT ( 'NONE',  ( -71.24615306438080609, 109.6430948152292189, -15.00000000000001421 ) ) ;
#6666 = VERTEX_POINT ( 'NONE', #16022 ) ;
#6665 = CARTESIAN_POINT ( 'NONE',  ( -68.99615306438077766, 115.1073470881302541, -167.1454815528550739 ) ) ;
#6667 = CARTESIAN_POINT ( 'NONE',  ( -115.7702289486887963, -95.65021661331553560, 5.654315315325360913 ) ) ;
#6668 = CARTESIAN_POINT ( 'NONE',  ( -71.24615306438091977, 75.97444640456376419, -15.00000000000001421 ) ) ;
#6669 = EDGE_LOOP ( 'NONE', ( #11604, #9846, #16670, #8571 ) ) ;
#6670 = CIRCLE ( 'NONE', #997, 4.000000000000024869 ) ;
#6671 = LINE ( 'NONE', #9853, #2648 ) ;
#6672 = ORIENTED_EDGE ( 'NONE', *, *, #11265, .F. ) ;
#6673 = EDGE_CURVE ( 'NONE', #17240, #16781, #3205, .T. ) ;
#6674 = AXIS2_PLACEMENT_3D ( 'NONE', #9595, #2490, #15299 ) ;
#6675 = VECTOR ( 'NONE', #12640, 1000.000000000000114 ) ;
#6676 = ORIENTED_EDGE ( 'NONE', *, *, #12311, .F. ) ;
#6677 = FACE_OUTER_BOUND ( 'NONE', #11850, .T. ) ;
#6678 = DIRECTION ( 'NONE',  ( -0.000000000000000000, -1.000000000000000000, -0.000000000000000000 ) ) ;
#6679 = DIRECTION ( 'NONE',  ( 1.000000000000000000, 0.000000000000000000, 5.551115123125786646E-16 ) ) ;
#6680 = ORIENTED_EDGE ( 'NONE', *, *, #1612, .T. ) ;
#6681 = PRODUCT_CONTEXT ( 'NONE', #17202, 'mechanical' ) ;
#6682 = DIRECTION ( 'NONE',  ( 0.000000000000000000, 1.000000000000000000, 0.000000000000000000 ) ) ;
#6683 = FACE_OUTER_BOUND ( 'NONE', #1744, .T. ) ;
#6684 = ORIENTED_EDGE ( 'NONE', *, *, #10304, .F. ) ;
#6685 = CARTESIAN_POINT ( 'NONE',  ( -68.99615306438077766, 123.9172691816626610, -15.00000000000001421 ) ) ;
#6686 = CYLINDRICAL_SURFACE ( 'NONE', #5415, 81.86696747278379860 ) ;
#6687 = DIRECTION ( 'NONE',  ( -1.000000000000000000, 0.000000000000000000, 0.000000000000000000 ) ) ;
#6688 = ORIENTED_EDGE ( 'NONE', *, *, #1689, .T. ) ;
#6689 = AXIS2_PLACEMENT_3D ( 'NONE', #14283, #15946, #4436 ) ;
#6690 = DIRECTION ( 'NONE',  ( -1.000000000000000000, 0.000000000000000000, 0.000000000000000000 ) ) ;
#6691 = DIRECTION ( 'NONE',  ( -1.000000000000000000, 0.000000000000000000, 0.000000000000000000 ) ) ;
#6692 = DIRECTION ( 'NONE',  ( 0.000000000000000000, 0.000000000000000000, -1.000000000000000000 ) ) ;
#6693 = VECTOR ( 'NONE', #6106, 1000.000000000000000 ) ;
#6694 = LINE ( 'NONE', #2590, #4895 ) ;
#6695 = VERTEX_POINT ( 'NONE', #13319 ) ;
#6696 = VECTOR ( 'NONE', #17485, 1000.000000000000000 ) ;
#6697 = AXIS2_PLACEMENT_3D ( 'NONE', #262, #14488, #3429 ) ;
#6698 = AXIS2_PLACEMENT_3D ( 'NONE', #4604, #14528, #8642 ) ;
#6699 = PRODUCT_DEFINITION_SHAPE ( 'NONE', 'NONE',  #6568 ) ;
#6700 = ORIENTED_EDGE ( 'NONE', *, *, #8492, .T. ) ;
#6701 = CARTESIAN_POINT ( 'NONE',  ( -60.71187100093244737, 74.64462966772953223, -15.00000000000001421 ) ) ;
#6702 = CARTESIAN_POINT ( 'NONE',  ( -71.24615306438083451, 97.96559495456375544, -167.1454815528550739 ) ) ;
#6703 = ORIENTED_EDGE ( 'NONE', *, *, #13922, .T. ) ;
#6704 = DIRECTION ( 'NONE',  ( -1.000000000000000000, 0.000000000000000000, 1.156482317317869999E-16 ) ) ;
#6705 = CARTESIAN_POINT ( 'NONE',  ( -78.08891603537360027, 82.99614312904147084, 55.09779029373265047 ) ) ;
#6706 = CARTESIAN_POINT ( 'NONE',  ( -68.99615306438111872, 7.678341131662685726, -167.1454815528550739 ) ) ;
#6707 = FACE_OUTER_BOUND ( 'NONE', #5046, .T. ) ;
#6708 = ORIENTED_EDGE ( 'NONE', *, *, #7357, .T. ) ;
#6709 = ADVANCED_FACE ( 'NONE', ( #13496 ), #679, .T. ) ;
#6710=STYLED_ITEM('',(#18545),#152);
#6711 = CARTESIAN_POINT ( 'NONE',  ( -53.53072411395612562, 94.43552448259771381, -167.1454815528550739 ) ) ;
#6712 = DIRECTION ( 'NONE',  ( 0.000000000000000000, 1.000000000000000000, 0.000000000000000000 ) ) ;
#6713 = CARTESIAN_POINT ( 'NONE',  ( -68.99615306438077766, 111.3508985816626335, 15.00000000000006928 ) ) ;
#6714 = CARTESIAN_POINT ( 'NONE',  ( -78.12361985383350316, 84.22855780814606419, 77.50000000000000000 ) ) ;
#6715 = DIRECTION ( 'NONE',  ( 0.000000000000000000, 0.000000000000000000, 1.000000000000000000 ) ) ;
#6716 = ORIENTED_EDGE ( 'NONE', *, *, #8992, .F. ) ;
#6717 = VECTOR ( 'NONE', #4451, 1000.000000000000000 ) ;
#6718 = AXIS2_PLACEMENT_3D ( 'NONE', #7265, #18498, #16800 ) ;
#6719 = AXIS2_PLACEMENT_3D ( 'NONE', #11871, #3630, #11962 ) ;
#6720 = CARTESIAN_POINT ( 'NONE',  ( -68.99615306438117557, 4.536748481662661980, -15.00000000000001421 ) ) ;
#6721 = DIRECTION ( 'NONE',  ( 0.9396926207859078728, 0.3420201433256701007, -1.086737899652989152E-16 ) ) ;
#6722 = ORIENTED_EDGE ( 'NONE', *, *, #8492, .F. ) ;
#6723 = CARTESIAN_POINT ( 'NONE',  ( -57.08002265617300708, 106.8109350805793270, 25.00000000000000355 ) ) ;
#6724 = CARTESIAN_POINT ( 'NONE',  ( -36.04074584300169448, 83.73612801793909455, 69.98790387965719617 ) ) ;
#6725 = EDGE_LOOP ( 'NONE', ( #16733, #17473, #2172, #15925 ) ) ;
#6726 = VERTEX_POINT ( 'NONE', #9196 ) ;
#6727 = AXIS2_PLACEMENT_3D ( 'NONE', #10392, #14869, #17311 ) ;
#6728 = VERTEX_POINT ( 'NONE', #16191 ) ;
#6729 = AXIS2_PLACEMENT_3D ( 'NONE', #2760, #14177, #1367 ) ;
#6730 = AXIS2_PLACEMENT_3D ( 'NONE', #5780, #8783, #11511 ) ;
#6731 = DIRECTION ( 'NONE',  ( -0.7071067811865474617, 8.659560562354932858E-17, -0.7071067811865474617 ) ) ;
#6732 = FACE_OUTER_BOUND ( 'NONE', #11099, .T. ) ;
#6733 = DIRECTION ( 'NONE',  ( 1.000000000000000000, 2.062304371594500740E-16, 0.000000000000000000 ) ) ;
#6734 = DIRECTION ( 'NONE',  ( -1.000000000000000000, -1.119176436114069332E-16, 0.000000000000000000 ) ) ;
#6735 = DIRECTION ( 'NONE',  ( 1.000000000000000000, 0.000000000000000000, 0.000000000000000000 ) ) ;
#6736 = DIRECTION ( 'NONE',  ( 0.000000000000000000, 0.000000000000000000, 1.000000000000000000 ) ) ;
#6737 = CARTESIAN_POINT ( 'NONE',  ( -92.59262256747319952, 50.58224449241410525, -35.00000000000000000 ) ) ;
#6738 = EDGE_LOOP ( 'NONE', ( #2454, #2015, #6381, #6161 ) ) ;
#6739 = DIRECTION ( 'NONE',  ( -0.9396926207859097602, 0.3420201433256649937, 0.000000000000000000 ) ) ;
#6740 = CARTESIAN_POINT ( 'NONE',  ( -57.08002265617300708, 84.22855780814606419, -62.50000000000000000 ) ) ;
#6741 = VERTEX_POINT ( 'NONE', #579 ) ;
#6742 = EDGE_CURVE ( 'NONE', #7250, #18326, #7167, .T. ) ;
#6743 = LINE ( 'NONE', #5044, #9727 ) ;
#6744 = AXIS2_PLACEMENT_3D ( 'NONE', #9234, #630, #4831 ) ;
#6745 = DIRECTION ( 'NONE',  ( 1.000000000000000000, 0.000000000000000000, 0.000000000000000000 ) ) ;
#6747 = EDGE_LOOP ( 'NONE', ( #1282, #3145, #8482, #14268 ) ) ;
#6746 = AXIS2_PLACEMENT_3D ( 'NONE', #13012, #187, #1946 ) ;
#6748 = VERTEX_POINT ( 'NONE', #6176 ) ;
#6749 = VERTEX_POINT ( 'NONE', #13129 ) ;
#6750 = EDGE_CURVE ( 'NONE', #1922, #4543, #5089, .T. ) ;
#6751 = DIRECTION ( 'NONE',  ( -0.000000000000000000, -0.000000000000000000, -1.000000000000000000 ) ) ;
#6752 = DIRECTION ( 'NONE',  ( 1.156482317317869999E-16, 0.000000000000000000, 1.000000000000000000 ) ) ;
#6753 = ADVANCED_FACE ( 'NONE', ( #3381 ), #4691, .T. ) ;
#6754 = FACE_OUTER_BOUND ( 'NONE', #6592, .T. ) ;
#6755 = CARTESIAN_POINT ( 'NONE',  ( -68.99615306438086293, 93.11619853813030545, -167.1454815528550739 ) ) ;
#6756 = ADVANCED_FACE ( 'NONE', ( #6367 ), #9010, .T. ) ;
#6757 = DIRECTION ( 'NONE',  ( -1.000000000000000000, 0.000000000000000000, 0.000000000000000000 ) ) ;
#6758 = LINE ( 'NONE', #1146, #9015 ) ;
#6759 = ORIENTED_EDGE ( 'NONE', *, *, #1176, .T. ) ;
#6760 = DIRECTION ( 'NONE',  ( 0.000000000000000000, 0.000000000000000000, -1.000000000000000000 ) ) ;
#6761 = CARTESIAN_POINT ( 'NONE',  ( -68.99615306438100504, 48.51904558166270220, -15.00000000000001421 ) ) ;
#6763 = ORIENTED_EDGE ( 'NONE', *, *, #9851, .F. ) ;
#6762 = CARTESIAN_POINT ( 'NONE',  ( -77.13858828394022282, 90.59309441108072747, 66.47525235387308840 ) ) ;
#6764 = CARTESIAN_POINT ( 'NONE',  ( -67.59262256747317110, 57.88796029049329661, -26.35917033480641436 ) ) ;
#6765 = DIRECTION ( 'NONE',  ( 0.9396926207859084279, 0.3420201433256686574, 0.000000000000000000 ) ) ;
#6766 = EDGE_LOOP ( 'NONE', ( #13502, #13833, #4409, #8667 ) ) ;
#6767 = EDGE_CURVE ( 'NONE', #4422, #16032, #13400, .T. ) ;
#6768 = EDGE_CURVE ( 'NONE', #7404, #60, #17416, .T. ) ;
#6769 = ADVANCED_FACE ( 'NONE', ( #11825 ), #9106, .F. ) ;
#6770 = CARTESIAN_POINT ( 'NONE',  ( -107.5926225674731711, 57.88796029049330372, 30.35917033480640370 ) ) ;
#6771 = ORIENTED_EDGE ( 'NONE', *, *, #14973, .T. ) ;
#6772 = EDGE_CURVE ( 'NONE', #2297, #10978, #10329, .T. ) ;
#6773 = ORIENTED_EDGE ( 'NONE', *, *, #3691, .F. ) ;
#6774 = FILL_AREA_STYLE_COLOUR ( '', #8207 ) ;
#6775 = CARTESIAN_POINT ( 'NONE',  ( -71.24615306438097662, 63.40807580456375803, -167.1454815528550739 ) ) ;
#6776 = DIRECTION ( 'NONE',  ( 0.000000000000000000, 1.000000000000000000, 0.000000000000000000 ) ) ;
#6777 = EDGE_LOOP ( 'NONE', ( #3979, #8991, #4544, #15238 ) ) ;
#6778 = EDGE_CURVE ( 'NONE', #6388, #10149, #11976, .T. ) ;
#6779 = CARTESIAN_POINT ( 'NONE',  ( -18.64094200358713493, 47.00521434539033550, -29.29675916631614285 ) ) ;
#6780 = EDGE_CURVE ( 'NONE', #1253, #535, #1897, .T. ) ;
#6781 = DIRECTION ( 'NONE',  ( -1.000000000000000000, 0.000000000000000000, -3.469446951953611033E-15 ) ) ;
#6782 = ORIENTED_EDGE ( 'NONE', *, *, #2041, .T. ) ;
#6783 = DIRECTION ( 'NONE',  ( 0.9475106458593564041, 0.3197242186372270534, 0.000000000000000000 ) ) ;
#6784 = DIRECTION ( 'NONE',  ( 0.000000000000000000, 0.000000000000000000, -1.000000000000000000 ) ) ;
#6785 = DIRECTION ( 'NONE',  ( 0.000000000000000000, 0.000000000000000000, -1.000000000000000000 ) ) ;
#6786 = ORIENTED_EDGE ( 'NONE', *, *, #14303, .F. ) ;
#6787 = CARTESIAN_POINT ( 'NONE',  ( -49.65031598894605480, 92.07579602767992810, 15.00000000000006928 ) ) ;
#6788 = CARTESIAN_POINT ( 'NONE',  ( -52.55467279550843784, 75.03273214436886462, -167.1454815528550739 ) ) ;
#6789 = ORIENTED_EDGE ( 'NONE', *, *, #8349, .F. ) ;
#6790 = DIRECTION ( 'NONE',  ( 1.000000000000000000, 0.000000000000000000, 0.000000000000000000 ) ) ;
#6791 = DIRECTION ( 'NONE',  ( -1.000000000000000000, 0.000000000000000000, -0.000000000000000000 ) ) ;
#6792 = ORIENTED_EDGE ( 'NONE', *, *, #13278, .F. ) ;
#6793 = EDGE_LOOP ( 'NONE', ( #8269, #16846, #14285 ) ) ;
#6794 = ORIENTED_EDGE ( 'NONE', *, *, #18024, .T. ) ;
#6795 = FACE_OUTER_BOUND ( 'NONE', #10659, .T. ) ;
#6796 = DIRECTION ( 'NONE',  ( 1.000000000000000000, 0.000000000000000000, 0.000000000000000000 ) ) ;
#6797 = ORIENTED_EDGE ( 'NONE', *, *, #12858, .T. ) ;
#6798 = DIRECTION ( 'NONE',  ( 0.000000000000000000, 1.000000000000000000, 0.000000000000000000 ) ) ;
#6799 = CARTESIAN_POINT ( 'NONE',  ( -42.53669312409158465, -96.08423613455721579, -10.65431531532567533 ) ) ;
#6800 = CARTESIAN_POINT ( 'NONE',  ( -15.48721883272544275, 31.28870489046039438, 38.35419603998612814 ) ) ;
#6801 = CARTESIAN_POINT ( 'NONE',  ( -92.59262256747319952, 57.88796029049330372, 26.35917033480641436 ) ) ;
#6802 = ORIENTED_EDGE ( 'NONE', *, *, #5511, .F. ) ;
#6803 = DIRECTION ( 'NONE',  ( 0.000000000000000000, 1.000000000000000000, 0.000000000000000000 ) ) ;
#6804 = DIRECTION ( 'NONE',  ( 0.000000000000000000, 0.000000000000000000, 1.000000000000000000 ) ) ;
#6805 = FACE_OUTER_BOUND ( 'NONE', #13102, .T. ) ;
#6806 = CYLINDRICAL_SURFACE ( 'NONE', #14124, 4.599999999999999645 ) ;
#6807 = DIRECTION ( 'NONE',  ( 0.3420201433256649937, -0.9396926207859097602, 0.000000000000000000 ) ) ;
#6808 = ORIENTED_EDGE ( 'NONE', *, *, #6181, .T. ) ;
#6809 = DIRECTION ( 'NONE',  ( -0.9396926207859158664, 0.3420201433256481738, 0.000000000000000000 ) ) ;
#6810 = CARTESIAN_POINT ( 'NONE',  ( -65.00992063631021267, -95.23217577251026000, 44.98760859132568868 ) ) ;
#6811 = CARTESIAN_POINT ( 'NONE',  ( -127.5926225674732279, 117.8748711238780373, 15.00000000000004263 ) ) ;
#6812 = CARTESIAN_POINT ( 'NONE',  ( -36.03642545851251100, 84.22855780814606419, 70.00000000000001421 ) ) ;
#6813 = ORIENTED_EDGE ( 'NONE', *, *, #5843, .F. ) ;
#6814 = EDGE_CURVE ( 'NONE', #7359, #8149, #10209, .T. ) ;
#6815 = EDGE_LOOP ( 'NONE', ( #10062, #14543, #6399, #14736 ) ) ;
#6816 = FACE_OUTER_BOUND ( 'NONE', #2715, .T. ) ;
#6817 = ADVANCED_FACE ( 'NONE', ( #17592 ), #11725, .T. ) ;
#6818 = EDGE_LOOP ( 'NONE', ( #2036, #10513, #13781, #6063, #5897, #17819, #9337, #14846, #9289, #13240, #938, #16181, #1596, #231, #1392, #8251 ) ) ;
#6819 = CARTESIAN_POINT ( 'NONE',  ( -68.99615306438110451, 2.010011688130255436, 15.00000000000006928 ) ) ;
#6820 = CARTESIAN_POINT ( 'NONE',  ( -74.58996131697591636, 60.64882399698279869, 23.45497070566349507 ) ) ;
#6821 = AXIS2_PLACEMENT_3D ( 'NONE', #17800, #13233, #12192 ) ;
#6822 = LINE ( 'NONE', #1031, #15035 ) ;
#6823 = EDGE_LOOP ( 'NONE', ( #1139, #1643, #1542, #8140 ) ) ;
#6824 = CARTESIAN_POINT ( 'NONE',  ( -64.09025127992788384, 59.14618053571278722, 37.50000000000000000 ) ) ;
#6825 = CARTESIAN_POINT ( 'NONE',  ( -42.21392442226139252, 53.23479276110153791, 25.06499217785701461 ) ) ;
#6826 = DIRECTION ( 'NONE',  ( -1.000000000000000000, 0.000000000000000000, 0.000000000000000000 ) ) ;
#6827 = ORIENTED_EDGE ( 'NONE', *, *, #3878, .F. ) ;
#6828 = CARTESIAN_POINT ( 'NONE',  ( -70.06856178257687873, 57.88796029049330372, -22.35917033480642502 ) ) ;
#6829 = CARTESIAN_POINT ( 'NONE',  ( -52.17699016282484337, 93.22868410554724505, -167.1454815528550739 ) ) ;
#6830 = VERTEX_POINT ( 'NONE', #5257 ) ;
#6831 = CARTESIAN_POINT ( 'NONE',  ( 124.5381772159375942, -46.83756720124470263, -115.7605492041889619 ) ) ;
#6832 = DIRECTION ( 'NONE',  ( -2.062304371594500494E-16, 1.000000000000000000, -0.000000000000000000 ) ) ;
#6833 = EDGE_LOOP ( 'NONE', ( #11883, #1404, #7842, #6844 ) ) ;
#6834 = AXIS2_PLACEMENT_3D ( 'NONE', #6079, #17862, #3194 ) ;
#6835 = ORIENTED_EDGE ( 'NONE', *, *, #7739, .F. ) ;
#6836 = EDGE_LOOP ( 'NONE', ( #1013, #10120, #4164, #5118 ) ) ;
#6837 = CARTESIAN_POINT ( 'NONE',  ( -68.99615306438067819, 143.3816809381303585, -167.1454815528550739 ) ) ;
#6838 = CARTESIAN_POINT ( 'NONE',  ( -71.24615306438109030, 31.99214930456376038, -15.00000000000001421 ) ) ;
#6839 = FACE_OUTER_BOUND ( 'NONE', #7942, .T. ) ;
#6840 = LINE ( 'NONE', #8049, #6654 ) ;
#6841 = EDGE_CURVE ( 'NONE', #3187, #9439, #777, .T. ) ;
#6842 = CARTESIAN_POINT ( 'NONE',  ( -46.27380910617147691, 84.15481808402802244, -15.00000000000001421 ) ) ;
#6843 = CARTESIAN_POINT ( 'NONE',  ( -60.31105839772099841, 93.95493478196522119, 15.00000000000006928 ) ) ;
#6844 = ORIENTED_EDGE ( 'NONE', *, *, #13958, .F. ) ;
#6845 = CIRCLE ( 'NONE', #12848, 11.04359719766049430 ) ;
#6846 = CARTESIAN_POINT ( 'NONE',  ( -71.24615306438091977, 78.22716831522920700, 15.00000000000006928 ) ) ;
#6847 = LINE ( 'NONE', #963, #9611 ) ;
#6849 = ORIENTED_EDGE ( 'NONE', *, *, #15471, .T. ) ;
#6848 = CARTESIAN_POINT ( 'NONE',  ( -77.86214395528257626, 87.56725157785864155, 69.23390454379837422 ) ) ;
#6850 = DIRECTION ( 'NONE',  ( -0.000000000000000000, 0.000000000000000000, 1.000000000000000000 ) ) ;
#6851 = CARTESIAN_POINT ( 'NONE',  ( -123.4618227840623632, -111.0842361345572158, -35.99999999999997158 ) ) ;
#6852 = VERTEX_POINT ( 'NONE', #13968 ) ;
#6853 = CARTESIAN_POINT ( 'NONE',  ( -68.99615306438111872, 8.293196988130274505, -167.1454815528550739 ) ) ;
#6854 = ORIENTED_EDGE ( 'NONE', *, *, #11891, .F. ) ;
#6855 = ADVANCED_FACE ( 'NONE', ( #13875 ), #11166, .T. ) ;
#6856 = EDGE_CURVE ( 'NONE', #16652, #2059, #2346, .T. ) ;
#6857 = AXIS2_PLACEMENT_3D ( 'NONE', #7791, #6373, #3386 ) ;
#6858 = ORIENTED_EDGE ( 'NONE', *, *, #3868, .F. ) ;
#6859 = VECTOR ( 'NONE', #13074, 1000.000000000000114 ) ;
#6860 = CARTESIAN_POINT ( 'NONE',  ( -69.66239992860627694, 84.22855780814606419, 37.50000000000000000 ) ) ;
#6861 = FACE_OUTER_BOUND ( 'NONE', #4067, .T. ) ;
#6862 = CARTESIAN_POINT ( 'NONE',  ( -81.37409655828237476, -91.08423613455721579, -28.18308811886549847 ) ) ;
#6863 = EDGE_CURVE ( 'NONE', #13855, #14048, #3762, .T. ) ;
#6864 = ORIENTED_EDGE ( 'NONE', *, *, #7898, .T. ) ;
#6865 = PRODUCT_CONTEXT ( 'NONE', #2503, 'mechanical' ) ;
#6866 = EDGE_CURVE ( 'NONE', #7744, #5248, #13205, .T. ) ;
#6867 = VERTEX_POINT ( 'NONE', #7967 ) ;
#6868 = CARTESIAN_POINT ( 'NONE',  ( -21.99673296352410645, 49.28519306194654348, -27.79101546118255328 ) ) ;
#6869 = LINE ( 'NONE', #10054, #1353 ) ;
#6870 = VERTEX_POINT ( 'NONE', #15162 ) ;
#6871 = DIRECTION ( 'NONE',  ( 0.000000000000000000, 0.000000000000000000, 1.000000000000000000 ) ) ;
#6872 = CYLINDRICAL_SURFACE ( 'NONE', #15270, 9.999999999999994671 ) ;
#6873 = DIRECTION ( 'NONE',  ( 1.000000000000000000, 2.062304371594500494E-16, 0.000000000000000000 ) ) ;
#6874 = ORIENTED_EDGE ( 'NONE', *, *, #1402, .T. ) ;
#6875 = VECTOR ( 'NONE', #16277, 1000.000000000000000 ) ;
#6876 = CARTESIAN_POINT ( 'NONE',  ( -70.87062273247055089, 110.1621498490178226, -22.37384807337301496 ) ) ;
#6877 = CARTESIAN_POINT ( 'NONE',  ( -7.405446926806058452E-14, -91.08423613455721579, 10.65431531532616560 ) ) ;
#6878 = ORIENTED_EDGE ( 'NONE', *, *, #5236, .T. ) ;
#6879 = EDGE_CURVE ( 'NONE', #565, #10632, #4261, .T. ) ;
#6880 = DIRECTION ( 'NONE',  ( -0.9913829028483789330, -0.1309959539066817280, 0.000000000000000000 ) ) ;
#6881 = EDGE_CURVE ( 'NONE', #11425, #17887, #14110, .T. ) ;
#6882 = CARTESIAN_POINT ( 'NONE',  ( -66.14871330646369074, 56.29489271423182828, -26.09800720142019159 ) ) ;
#6883 = ORIENTED_EDGE ( 'NONE', *, *, #10741, .T. ) ;
#6884 = ADVANCED_FACE ( 'NONE', ( #7878 ), #13774, .T. ) ;
#6885 = EDGE_CURVE ( 'NONE', #6195, #5943, #10490, .T. ) ;
#6886 = ORIENTED_EDGE ( 'NONE', *, *, #13513, .F. ) ;
#6887 = CIRCLE ( 'NONE', #9886, 29.36884788726140627 ) ;
#6888 = DIRECTION ( 'NONE',  ( 0.000000000000000000, 0.000000000000000000, 1.000000000000000000 ) ) ;
#6889 = EDGE_CURVE ( 'NONE', #15247, #2633, #6663, .T. ) ;
#6890 = ORIENTED_EDGE ( 'NONE', *, *, #12118, .F. ) ;
#6891 = VECTOR ( 'NONE', #2241, 1000.000000000000000 ) ;
#6892 = DIRECTION ( 'NONE',  ( 0.9396926207859084279, 0.3420201433256686574, 4.890320548438448905E-16 ) ) ;
#6893 = DIRECTION ( 'NONE',  ( 0.000000000000000000, 0.8660254037844387076, 0.4999999999999999445 ) ) ;
#6894 = AXIS2_PLACEMENT_3D ( 'NONE', #11026, #15131, #829 ) ;
#6895 = DIRECTION ( 'NONE',  ( 0.000000000000000000, 1.000000000000000000, 0.000000000000000000 ) ) ;
#6896 = VERTEX_POINT ( 'NONE', #15262 ) ;
#6897 = DIRECTION ( 'NONE',  ( 1.000000000000000000, 0.000000000000000000, 0.000000000000000000 ) ) ;
#6898 = PLANE ( 'NONE',  #13039 ) ;
#6899 = CARTESIAN_POINT ( 'NONE',  ( -75.86129610575210336, 106.8071537307722991, 25.00000000000000355 ) ) ;
#6900 = PLANE ( 'NONE',  #3941 ) ;
#6901 = CARTESIAN_POINT ( 'NONE',  ( 5.099753278416039315, 20.30794007945024759, 43.46515485487502417 ) ) ;
#6902 = VERTEX_POINT ( 'NONE', #6465 ) ;
#6903 = MECHANICAL_DESIGN_GEOMETRIC_PRESENTATION_REPRESENTATION (  '', ( #15852 ), #8691 ) ;
#6904 = DIRECTION ( 'NONE',  ( 0.000000000000000000, 0.000000000000000000, 1.000000000000000000 ) ) ;
#6905 = DIRECTION ( 'NONE',  ( 0.7930648017909424086, 0.6091372753003162499, 5.105014369306161237E-16 ) ) ;
#6906 = VECTOR ( 'NONE', #18424, 1000.000000000000000 ) ;
#6907 = CARTESIAN_POINT ( 'NONE',  ( -68.99615306438077766, 114.4924912316626688, 15.00000000000006928 ) ) ;
#6908 = CIRCLE ( 'NONE', #12272, 22.04359719766050318 ) ;
#6909 = CARTESIAN_POINT ( 'NONE',  ( -71.24615306438089135, 82.25763170456374951, -167.1454815528550739 ) ) ;
#6910 = ORIENTED_EDGE ( 'NONE', *, *, #16367, .T. ) ;
#6911 = VERTEX_POINT ( 'NONE', #17876 ) ;
#6912 = DIRECTION ( 'NONE',  ( -0.000000000000000000, -0.000000000000000000, -1.000000000000000000 ) ) ;
#6913 = CIRCLE ( 'NONE', #8998, 4.599999999999999645 ) ;
#6914 = VERTEX_POINT ( 'NONE', #16473 ) ;
#6915 = LINE ( 'NONE', #9815, #3142 ) ;
#6916 = DIRECTION ( 'NONE',  ( -1.000000000000000000, -0.000000000000000000, -0.000000000000000000 ) ) ;
#6917 = LINE ( 'NONE', #1576, #6081 ) ;
#6918 = ORIENTED_EDGE ( 'NONE', *, *, #3317, .T. ) ;
#6919 = LINE ( 'NONE', #4206, #7772 ) ;
#6920 = AXIS2_PLACEMENT_3D ( 'NONE', #15863, #3052, #6021 ) ;
#6921 = AXIS2_PLACEMENT_3D ( 'NONE', #18476, #5647, #4252 ) ;
#6922 = CARTESIAN_POINT ( 'NONE',  ( 0.2578475836320668346, 6.890627091270365767, 1.065083781909175187 ) ) ;
#6923 = CARTESIAN_POINT ( 'NONE',  ( -57.08002265617300708, 84.22855780814606419, -62.50000000000000000 ) ) ;
#6924 = DIRECTION ( 'NONE',  ( 1.000000000000000000, 0.000000000000000000, 0.000000000000000000 ) ) ;
#6925 = ORIENTED_EDGE ( 'NONE', *, *, #1499, .T. ) ;
#6926 = PRODUCT_RELATED_PRODUCT_CATEGORY ( 'part', '', ( #2532 ) ) ;
#6927 = FACE_OUTER_BOUND ( 'NONE', #11643, .T. ) ;
#6928 = VERTEX_POINT ( 'NONE', #6846 ) ;
#6929 = AXIS2_PLACEMENT_3D ( 'NONE', #6557, #5439, #10777 ) ;
#6930 = DIRECTION ( 'NONE',  ( 1.000000000000000000, 0.000000000000000000, 0.000000000000000000 ) ) ;
#6931 = DIRECTION ( 'NONE',  ( 1.119176436114069332E-16, -1.000000000000000000, -0.000000000000000000 ) ) ;
#6932 = EDGE_LOOP ( 'NONE', ( #14224, #6874 ) ) ;
#6933 = APPLICATION_CONTEXT ( 'automotive_design' ) ;
#6934 = VERTEX_POINT ( 'NONE', #12385 ) ;
#6935 = CIRCLE ( 'NONE', #18285, 29.36884788726140627 ) ;
#6936 = AXIS2_PLACEMENT_3D ( 'NONE', #14153, #12765, #5628 ) ;
#6937 = VERTEX_POINT ( 'NONE', #9556 ) ;
#6938 = CARTESIAN_POINT ( 'NONE',  ( -70.27900850916093134, -2.213358015103445098, -15.00000000000001599 ) ) ;
#6939 = CARTESIAN_POINT ( 'NONE',  ( -42.53669312409158465, -91.08423613455721579, 5.204170427930421283E-15 ) ) ;
#6940 = FACE_OUTER_BOUND ( 'NONE', #12701, .T. ) ;
#6941 = B_SPLINE_CURVE_WITH_KNOTS ( 'NONE', 3,
 ( #8567, #7073, #7414, #5998, #11726, #8918 ),
 .UNSPECIFIED., .F., .F.,
 ( 4, 2, 4 ),
 ( 2.380733003239153451E-07, 0.001898835937927371162, 0.003797433802554418120 ),
 .UNSPECIFIED. ) ;
#6942 = CIRCLE ( 'NONE', #17377, 12.58237727243326987 ) ;
#6943 = DIRECTION ( 'NONE',  ( 0.000000000000000000, 1.000000000000000000, 0.000000000000000000 ) ) ;
#6944 = CARTESIAN_POINT ( 'NONE',  ( 0.5805565836007609004, 3.752776749732559924, -6.500000000000061284 ) ) ;
#6945 = ORIENTED_EDGE ( 'NONE', *, *, #7574, .F. ) ;
#6946 = ADVANCED_FACE ( 'NONE', ( #15368 ), #12281, .T. ) ;
#6947 = CARTESIAN_POINT ( 'NONE',  ( -51.85133027979232878, 95.58244595420329404, -15.00000000000001421 ) ) ;
#6948 = ORIENTED_EDGE ( 'NONE', *, *, #1401, .F. ) ;
#6949 = CARTESIAN_POINT ( 'NONE',  ( -107.5926225674731853, 110.5691553257988460, 26.35917033480641436 ) ) ;
#6950 = VECTOR ( 'NONE', #13448, 1000.000000000000000 ) ;
#6951 = AXIS2_PLACEMENT_3D ( 'NONE', #1491, #3171, #11681 ) ;
#6952 = LINE ( 'NONE', #5065, #8378 ) ;
#6953 = ORIENTED_EDGE ( 'NONE', *, *, #717, .F. ) ;
#6954 = DIRECTION ( 'NONE',  ( -1.000000000000000000, -0.000000000000000000, -0.000000000000000000 ) ) ;
#6955 = VERTEX_POINT ( 'NONE', #2263 ) ;
#6956 = VECTOR ( 'NONE', #16766, 1000.000000000000114 ) ;
#6957 = EDGE_CURVE ( 'NONE', #14359, #17240, #5339, .T. ) ;
#6958 = VERTEX_POINT ( 'NONE', #12566 ) ;
#6959 = AXIS2_PLACEMENT_3D ( 'NONE', #3876, #12600, #15584 ) ;
#6960 = AXIS2_PLACEMENT_3D ( 'NONE', #12101, #780, #2351 ) ;
#6961 = LINE ( 'NONE', #7144, #10893 ) ;
#6962 = LINE ( 'NONE', #3960, #9991 ) ;
#6963 = DIRECTION ( 'NONE',  ( 1.000000000000000000, 2.062304371594500494E-16, 0.000000000000000000 ) ) ;
#6964 = ORIENTED_EDGE ( 'NONE', *, *, #10196, .T. ) ;
#6965 = ORIENTED_EDGE ( 'NONE', *, *, #17958, .F. ) ;
#6966 = CARTESIAN_POINT ( 'NONE',  ( -71.24615306438067819, 144.2006139652292518, -15.00000000000001421 ) ) ;
#6967 = DIRECTION ( 'NONE',  ( -5.204170427930409450E-16, 0.000000000000000000, 1.000000000000000000 ) ) ;
#6968 = EDGE_LOOP ( 'NONE', ( #9033, #15562, #7945, #621 ) ) ;
#6969 = CIRCLE ( 'NONE', #13830, 2.168074330098676672 ) ;
#6970 = LINE ( 'NONE', #5650, #10790 ) ;
#6971 = FACE_OUTER_BOUND ( 'NONE', #11554, .T. ) ;
#6972 = PLANE ( 'NONE',  #10525 ) ;
#6973 = ORIENTED_EDGE ( 'NONE', *, *, #2178, .T. ) ;
#6974 = DIRECTION ( 'NONE',  ( 1.000000000000000000, 0.000000000000000000, -0.000000000000000000 ) ) ;
#6975 = FACE_OUTER_BOUND ( 'NONE', #16067, .T. ) ;
#6976 = VERTEX_POINT ( 'NONE', #12185 ) ;
#6977 = AXIS2_PLACEMENT_3D ( 'NONE', #2140, #12246, #10567 ) ;
#6978 = VECTOR ( 'NONE', #2245, 1000.000000000000000 ) ;
#6979 = CARTESIAN_POINT ( 'NONE',  ( -49.58002265617300708, 84.22855780814606419, -35.00000000000000000 ) ) ;
#6980 = CIRCLE ( 'NONE', #17410, 172.7605492041889192 ) ;
#6981 = EDGE_CURVE ( 'NONE', #3596, #14710, #7504, .T. ) ;
#6982 = EDGE_CURVE ( 'NONE', #9400, #1024, #3316, .T. ) ;
#6983 = DIRECTION ( 'NONE',  ( 0.000000000000000000, 0.000000000000000000, 1.000000000000000000 ) ) ;
#6984 = VERTEX_POINT ( 'NONE', #16954 ) ;
#6985 = CIRCLE ( 'NONE', #15335, 10.24900000000001477 ) ;
#6986 = EDGE_LOOP ( 'NONE', ( #7391, #15536, #1783, #34 ) ) ;
#6987 = DIRECTION ( 'NONE',  ( 0.000000000000000000, 0.000000000000000000, -1.000000000000000000 ) ) ;
#6988 = DIRECTION ( 'NONE',  ( 1.000000000000000000, 0.000000000000000000, 0.000000000000000000 ) ) ;
#6989 = VERTEX_POINT ( 'NONE', #4408 ) ;
#6990 = AXIS2_PLACEMENT_3D ( 'NONE', #16050, #11510, #10093 ) ;
#6991 = EDGE_CURVE ( 'NONE', #3816, #17058, #17040, .T. ) ;
#6992 = VECTOR ( 'NONE', #5412, 1000.000000000000000 ) ;
#6993 = CARTESIAN_POINT ( 'NONE',  ( -71.24615306438080609, 115.9262801152292042, -167.1454815528550739 ) ) ;
#6995 = VECTOR ( 'NONE', #9570, 1000.000000000000114 ) ;
#6994 = CARTESIAN_POINT ( 'NONE',  ( -48.13268001719898592, 75.49957964911752129, 15.00000000000006928 ) ) ;
#6996 = DIRECTION ( 'NONE',  ( 0.9396926207859171987, 0.3420201433256444545, -1.086737899652999999E-16 ) ) ;
#6997 = ADVANCED_FACE ( 'NONE', ( #2644 ), #18371, .F. ) ;
#6998 = LINE ( 'NONE', #12620, #7609 ) ;
#6999 = VERTEX_POINT ( 'NONE', #1607 ) ;
#7000 = EDGE_CURVE ( 'NONE', #11655, #13953, #9603, .T. ) ;
#7001 = LINE ( 'NONE', #8400, #1806 ) ;
#7002 = DIRECTION ( 'NONE',  ( 0.9396926207859102043, 0.3420201433256637724, 0.000000000000000000 ) ) ;
#7003 = EDGE_CURVE ( 'NONE', #16011, #15896, #15823, .T. ) ;
#7004 = CARTESIAN_POINT ( 'NONE',  ( -11.55310279070829260, 26.82330587308622682, -40.51155826455459419 ) ) ;
#7005 = CARTESIAN_POINT ( 'NONE',  ( -71.24615306438107609, 31.99214930456376749, -15.00000000000001421 ) ) ;
#7006 = ORIENTED_EDGE ( 'NONE', *, *, #2156, .T. ) ;
#7007 = VECTOR ( 'NONE', #7083, 1000.000000000000000 ) ;
#7008 = DIRECTION ( 'NONE',  ( 0.000000000000000000, 0.000000000000000000, 1.000000000000000000 ) ) ;
#7009 = ADVANCED_FACE ( 'NONE', ( #14335 ), #5630, .T. ) ;
#7011 = EDGE_CURVE ( 'NONE', #3213, #13490, #1430, .T. ) ;
#7010 = PRODUCT_DEFINITION_FORMATION_WITH_SPECIFIED_SOURCE ( 'ANY', '', #13410, .NOT_KNOWN. ) ;
#7012 = DIRECTION ( 'NONE',  ( -0.000000000000000000, -0.000000000000000000, 1.000000000000000000 ) ) ;
#7013 = CIRCLE ( 'NONE', #124, 6.500000000000039968 ) ;
#7014 = EDGE_CURVE ( 'NONE', #7349, #1231, #16469, .T. ) ;
#7015 = DIRECTION ( 'NONE',  ( 0.000000000000000000, 1.000000000000000000, 0.000000000000000000 ) ) ;
#7016 = VERTEX_POINT ( 'NONE', #6947 ) ;
#7017 = CIRCLE ( 'NONE', #12072, 3.445500000000021767 ) ;
#7018 = ORIENTED_EDGE ( 'NONE', *, *, #5025, .F. ) ;
#7019 = EDGE_CURVE ( 'NONE', #1167, #18033, #8347, .T. ) ;
#7020 = PLANE ( 'NONE',  #13852 ) ;
#7021 = ORIENTED_EDGE ( 'NONE', *, *, #16353, .F. ) ;
#7022 = FACE_OUTER_BOUND ( 'NONE', #12284, .T. ) ;
#7023 = CARTESIAN_POINT ( 'NONE',  ( -68.99615306438111872, 14.57638228813026871, -167.1454815528550739 ) ) ;
#7024 = PLANE ( 'NONE',  #16230 ) ;
#7025 = ORIENTED_EDGE ( 'NONE', *, *, #12616, .F. ) ;
#7026 = CIRCLE ( 'NONE', #12997, 3.999999999999989786 ) ;
#7027 = CARTESIAN_POINT ( 'NONE',  ( -67.37304936704279612, 107.3218817776568130, -27.99999999999999645 ) ) ;
#7028 = AXIS2_PLACEMENT_3D ( 'NONE', #12119, #793, #12201 ) ;
#7029 = DIRECTION ( 'NONE',  ( -0.5150380749100570421, 1.049727191138616600E-16, -0.8571673007021106683 ) ) ;
#7030 = EDGE_CURVE ( 'NONE', #848, #10424, #11708, .T. ) ;
#7031 = DIRECTION ( 'NONE',  ( -1.000000000000000000, 0.000000000000000000, 0.000000000000000000 ) ) ;
#7032 = AXIS2_PLACEMENT_3D ( 'NONE', #6528, #10841, #12245 ) ;
#7033 = LINE ( 'NONE', #9449, #2776 ) ;
#7034 = VERTEX_POINT ( 'NONE', #11349 ) ;
#7035 = EDGE_CURVE ( 'NONE', #16976, #4613, #14059, .T. ) ;
#7036 = DIRECTION ( 'NONE',  ( 1.000000000000000000, 0.000000000000000000, 0.000000000000000000 ) ) ;
#7037 = ORIENTED_EDGE ( 'NONE', *, *, #3280, .F. ) ;
#7038 = AXIS2_PLACEMENT_3D ( 'NONE', #16014, #11621, #13123 ) ;
#7039 = FACE_OUTER_BOUND ( 'NONE', #11821, .T. ) ;
#7040 = LINE ( 'NONE', #12832, #8930 ) ;
#7041 = VERTEX_POINT ( 'NONE', #12767 ) ;
#7042 = EDGE_LOOP ( 'NONE', ( #17814, #1254, #11492, #8289 ) ) ;
#7043 = VECTOR ( 'NONE', #2968, 1000.000000000000000 ) ;
#7044 = AXIS2_PLACEMENT_3D ( 'NONE', #3266, #17568, #14948 ) ;
#7045 = AXIS2_PLACEMENT_3D ( 'NONE', #9144, #17742, #1937 ) ;
#7046 = ORIENTED_EDGE ( 'NONE', *, *, #9865, .T. ) ;
#7047 = PRODUCT_DEFINITION_CONTEXT ( 'detailed design', #2022, 'design' ) ;
#7048 = CARTESIAN_POINT ( 'NONE',  ( -70.71978124295696944, -141.5628872026273086, 5.204170427930421283E-15 ) ) ;
#7049 = CARTESIAN_POINT ( 'NONE',  ( -64.09025127992788384, 50.58224449241410525, 35.00000000000000000 ) ) ;
#7050 = PLANE ( 'NONE',  #870 ) ;
#7051 = DIRECTION ( 'NONE',  ( 0.000000000000000000, 0.000000000000000000, 1.000000000000000000 ) ) ;
#7052 = CARTESIAN_POINT ( 'NONE',  ( -71.24615306438106188, 34.24487121522926003, -167.1454815528550739 ) ) ;
#7053 = ORIENTED_EDGE ( 'NONE', *, *, #14696, .F. ) ;
#7054 = DIRECTION ( 'NONE',  ( -0.9396926207859084279, 0.3420201433256686574, 0.000000000000000000 ) ) ;
#7055 = ORIENTED_EDGE ( 'NONE', *, *, #6488, .F. ) ;
#7056 = CARTESIAN_POINT ( 'NONE',  ( -45.85876501399108207, 78.72098330317804482, -167.1454815528550739 ) ) ;
#7057 = AXIS2_PLACEMENT_3D ( 'NONE', #7556, #6507, #18321 ) ;
#7058 = FACE_OUTER_BOUND ( 'NONE', #1696, .T. ) ;
#7059 = ORIENTED_EDGE ( 'NONE', *, *, #17385, .F. ) ;
#7060 = CARTESIAN_POINT ( 'NONE',  ( -57.08002265617300708, 84.22855780814606419, 15.00000000000006928 ) ) ;
#7061 = VERTEX_POINT ( 'NONE', #5716 ) ;
#7062 = EDGE_CURVE ( 'NONE', #10261, #16893, #17360, .T. ) ;
#7063 = VERTEX_POINT ( 'NONE', #2736 ) ;
#7064 =( LENGTH_UNIT ( ) NAMED_UNIT ( * ) SI_UNIT ( .MILLI., .METRE. ) );
#7065 = CARTESIAN_POINT ( 'NONE',  ( -71.24615306438114715, 16.28418605456380419, -167.1454815528550739 ) ) ;
#7066 = FACE_OUTER_BOUND ( 'NONE', #14131, .T. ) ;
#7067 = ORIENTED_EDGE ( 'NONE', *, *, #16132, .F. ) ;
#7068 = ORIENTED_EDGE ( 'NONE', *, *, #18058, .F. ) ;
#7069 = CARTESIAN_POINT ( 'NONE',  ( -17.02762337565411244, 45.80709108728513712, -30.06585831480913740 ) ) ;
#7070 = CARTESIAN_POINT ( 'NONE',  ( -70.85175816390371040, -141.5628872026273086, -18.23991632971912225 ) ) ;
#7071 = EDGE_LOOP ( 'NONE', ( #4477, #13671, #8282, #9085 ) ) ;
#7072 = DIRECTION ( 'NONE',  ( 0.9396926207859134239, 0.3420201433256546686, 4.890320548438474543E-16 ) ) ;
#7073 = CARTESIAN_POINT ( 'NONE',  ( 0.4033376246893360939, -7.198601258567047800, 0.5316568767328908596 ) ) ;
#7074 = DIRECTION ( 'NONE',  ( 0.000000000000000000, 1.000000000000000000, 0.000000000000000000 ) ) ;
#7075 = ORIENTED_EDGE ( 'NONE', *, *, #2430, .F. ) ;
#7076 = DIRECTION ( 'NONE',  ( 1.000000000000000000, 0.000000000000000000, 0.000000000000000000 ) ) ;
#7077 = ORIENTED_EDGE ( 'NONE', *, *, #485, .F. ) ;
#7078 = ORIENTED_EDGE ( 'NONE', *, *, #9858, .F. ) ;
#7079 = CARTESIAN_POINT ( 'NONE',  ( -67.36171047226943642, 56.71715511495233386, -22.93244165942064683 ) ) ;
#7080 = ORIENTED_EDGE ( 'NONE', *, *, #11885, .T. ) ;
#7081 = ORIENTED_EDGE ( 'NONE', *, *, #1401, .T. ) ;
#7082 = EDGE_CURVE ( 'NONE', #3118, #12199, #9942, .T. ) ;
#7083 = DIRECTION ( 'NONE',  ( 0.9396926207859097602, 0.3420201433256649937, -1.086737899652991371E-16 ) ) ;
#7084 = FACE_OUTER_BOUND ( 'NONE', #12266, .T. ) ;
#7085 = CARTESIAN_POINT ( 'NONE',  ( 9.543663295069050534, 56.41207303426870112, 7.000000000000010658 ) ) ;
#7086 = ORIENTED_EDGE ( 'NONE', *, *, #15403, .F. ) ;
#7087 = FACE_OUTER_BOUND ( 'NONE', #2437, .T. ) ;
#7088 = CARTESIAN_POINT ( 'NONE',  ( -123.4618227840623632, -111.0842361345572158, 57.00000000000000000 ) ) ;
#7089 = DIRECTION ( 'NONE',  ( -1.000000000000000000, 2.220446049250314659E-15, 1.387778780781446662E-16 ) ) ;
#7090 = CARTESIAN_POINT ( 'NONE',  ( -71.24615306438097662, 62.51920506522922949, 15.00000000000006928 ) ) ;
#7091 = VERTEX_POINT ( 'NONE', #11442 ) ;
#7092 = ADVANCED_FACE ( 'NONE', ( #8445 ), #14156, .T. ) ;
#7093 = DIRECTION ( 'NONE',  ( 0.000000000000000000, 0.000000000000000000, 1.000000000000000000 ) ) ;
#7094 = CARTESIAN_POINT ( 'NONE',  ( -76.37409655828236055, -96.08423613455721579, -28.18308811886544873 ) ) ;
#7095 = PLANE ( 'NONE',  #11722 ) ;
#7096 = ORIENTED_EDGE ( 'NONE', *, *, #9621, .T. ) ;
#7097 = DIRECTION ( 'NONE',  ( -0.9396926207859069846, 0.3420201433256723766, 0.000000000000000000 ) ) ;
#7098 = CARTESIAN_POINT ( 'NONE',  ( -68.12361985383350316, 84.22855780814606419, 35.00000000000000000 ) ) ;
#7099 = LINE ( 'NONE', #18230, #12890 ) ;
#7100 = FACE_OUTER_BOUND ( 'NONE', #14223, .T. ) ;
#7101 = ORIENTED_EDGE ( 'NONE', *, *, #13741, .F. ) ;
#7102 = ADVANCED_FACE ( 'NONE', ( #18465 ), #14253, .F. ) ;
#7103 = ORIENTED_EDGE ( 'NONE', *, *, #6863, .F. ) ;
#7104 = EDGE_CURVE ( 'NONE', #14076, #12606, #2925, .T. ) ;
#7105 = CARTESIAN_POINT ( 'NONE',  ( -57.08002265617300708, 84.22855780814606419, 15.00000000000006928 ) ) ;
#7106 = ORIENTED_EDGE ( 'NONE', *, *, #5247, .T. ) ;
#7107 = CARTESIAN_POINT ( 'NONE',  ( -75.73737094285307592, 61.54687875405910091, 24.71467968727341713 ) ) ;
#7108 = DIRECTION ( 'NONE',  ( 1.000000000000000000, 0.000000000000000000, 0.000000000000000000 ) ) ;
#7109 = ORIENTED_EDGE ( 'NONE', *, *, #1163, .T. ) ;
#7110 = ADVANCED_FACE ( 'NONE', ( #3104 ), #4673, .T. ) ;
#7111 = ADVANCED_FACE ( 'NONE', ( #13204 ), #17397, .T. ) ;
#7112 = CARTESIAN_POINT ( 'NONE',  ( 113.3630170098443273, -111.0842361345571874, 7.000000000000010658 ) ) ;
#7113 = EDGE_CURVE ( 'NONE', #3601, #17247, #2748, .T. ) ;
#7114 = CARTESIAN_POINT ( 'NONE',  ( -70.71978124295696944, -91.08423613455721579, 5.204170427930421283E-15 ) ) ;
#7115 = FACE_OUTER_BOUND ( 'NONE', #16644, .T. ) ;
#7116 = CARTESIAN_POINT ( 'NONE',  ( -57.08002265617300708, 84.22855780814606419, 37.50000000000000000 ) ) ;
#7117 = ORIENTED_EDGE ( 'NONE', *, *, #13138, .F. ) ;
#7118 = CARTESIAN_POINT ( 'NONE',  ( -68.99615306438106188, 26.52789703166272162, -167.1454815528550739 ) ) ;
#7119 = EDGE_LOOP ( 'NONE', ( #16844, #7372 ) ) ;
#7120 = EDGE_CURVE ( 'NONE', #16262, #14197, #555, .T. ) ;
#7121 = CARTESIAN_POINT ( 'NONE',  ( -68.99615306438070661, 127.6737176881302958, -15.00000000000001421 ) ) ;
#7122 = LINE ( 'NONE', #5614, #1751 ) ;
#7123 = VERTEX_POINT ( 'NONE', #13300 ) ;
#7124 = VERTEX_POINT ( 'NONE', #479 ) ;
#7125 = ADVANCED_FACE ( 'NONE', ( #6609 ), #9311, .T. ) ;
#7126 = EDGE_CURVE ( 'NONE', #9885, #15640, #6074, .T. ) ;
#7127 = ORIENTED_EDGE ( 'NONE', *, *, #13514, .T. ) ;
#7128 = FACE_OUTER_BOUND ( 'NONE', #6986, .T. ) ;
#7129 = CARTESIAN_POINT ( 'NONE',  ( -59.20641439073742873, 73.63336328296978195, -15.00000000000001421 ) ) ;
#7130 = DIRECTION ( 'NONE',  ( 1.000000000000000000, 0.000000000000000000, 3.771137991253928573E-16 ) ) ;
#7131 = ADVANCED_FACE ( 'NONE', ( #3360 ), #6301, .F. ) ;
#7132 = DIRECTION ( 'NONE',  ( -1.000000000000000000, 6.033820786006295184E-15, 0.000000000000000000 ) ) ;
#7133 = CARTESIAN_POINT ( 'NONE',  ( -52.35105328106566702, 95.79950628479642205, 15.00000000000006928 ) ) ;
#7134 = ORIENTED_EDGE ( 'NONE', *, *, #5610, .T. ) ;
#7135 = CARTESIAN_POINT ( 'NONE',  ( 276.3098885457529832, -32.62665103886256190, 7.000000000000010658 ) ) ;
#7136 = VERTEX_POINT ( 'NONE', #14683 ) ;
#7137 = LINE ( 'NONE', #16657, #14713 ) ;
#7138 = DIRECTION ( 'NONE',  ( 0.3420201433256444545, -0.9396926207859171987, 0.000000000000000000 ) ) ;
#7139 = VECTOR ( 'NONE', #6832, 1000.000000000000000 ) ;
#7140 = ORIENTED_EDGE ( 'NONE', *, *, #7236, .F. ) ;
#7141 = CARTESIAN_POINT ( 'NONE',  ( -114.1362093120868337, -92.58100082067039693, -7.070573948081583460 ) ) ;
#7142 = VERTEX_POINT ( 'NONE', #13114 ) ;
#7143 = ORIENTED_EDGE ( 'NONE', *, *, #15921, .F. ) ;
#7144 = CARTESIAN_POINT ( 'NONE',  ( -71.24615306438109030, 31.10327856522923540, -167.1454815528550739 ) ) ;
#7145 = AXIS2_PLACEMENT_3D ( 'NONE', #14690, #12173, #3276 ) ;
#7146 = DIRECTION ( 'NONE',  ( 0.000000000000000000, 0.000000000000000000, 1.000000000000000000 ) ) ;
#7147 = LINE ( 'NONE', #1793, #17680 ) ;
#7148 = ORIENTED_EDGE ( 'NONE', *, *, #6051, .F. ) ;
#7149 = ORIENTED_EDGE ( 'NONE', *, *, #7406, .T. ) ;
#7150 = CYLINDRICAL_SURFACE ( 'NONE', #5215, 20.99999999999999645 ) ;
#7151 = VERTEX_POINT ( 'NONE', #14779 ) ;
#7152 = DIRECTION ( 'NONE',  ( 0.000000000000000000, 0.000000000000000000, 1.000000000000000000 ) ) ;
#7153 = DIRECTION ( 'NONE',  ( 0.000000000000000000, 0.000000000000000000, 1.000000000000000000 ) ) ;
#7154 = DIRECTION ( 'NONE',  ( -0.000000000000000000, 1.000000000000000000, -0.000000000000000000 ) ) ;
#7155 = VERTEX_POINT ( 'NONE', #17669 ) ;
#7156 = CARTESIAN_POINT ( 'NONE',  ( -50.41499038512538533, 117.9449492212793302, 0.000000000000000000 ) ) ;
#7157 = ORIENTED_EDGE ( 'NONE', *, *, #4770, .F. ) ;
#7158 = ORIENTED_EDGE ( 'NONE', *, *, #1456, .F. ) ;
#7159 = CIRCLE ( 'NONE', #13124, 1.000000000000000888 ) ;
#7160 = DIRECTION ( 'NONE',  ( -1.000000000000000000, -0.000000000000000000, -0.000000000000000000 ) ) ;
#7161 = VECTOR ( 'NONE', #5941, 1000.000000000000000 ) ;
#7162 = ORIENTED_EDGE ( 'NONE', *, *, #560, .T. ) ;
#7163 = CYLINDRICAL_SURFACE ( 'NONE', #14746, 12.50000000000000355 ) ;
#7164 = CARTESIAN_POINT ( 'NONE',  ( -127.5926225674731995, 47.87487112387803023, -15.00000000000000355 ) ) ;
#7165 = LINE ( 'NONE', #235, #3098 ) ;
#7166 = VERTEX_POINT ( 'NONE', #2055 ) ;
#7167 = B_SPLINE_CURVE_WITH_KNOTS ( 'NONE', 3,
 ( #8917, #12098, #7692, #7785, #10492, #16095 ),
 .UNSPECIFIED., .F., .F.,
 ( 4, 2, 4 ),
 ( 2.380733003370977718E-07, 0.001898835937927384606, 0.003797433802554432431 ),
 .UNSPECIFIED. ) ;
#7168 = DIRECTION ( 'NONE',  ( -1.000000000000000000, -0.000000000000000000, -0.000000000000000000 ) ) ;
#7169 = DIRECTION ( 'NONE',  ( 0.000000000000000000, 0.000000000000000000, 1.000000000000000000 ) ) ;
#7170 = CARTESIAN_POINT ( 'NONE',  ( -57.08002265617300708, 84.22855780814606419, -15.00000000000001421 ) ) ;
#7171 = CIRCLE ( 'NONE', #6232, 29.36884788726140627 ) ;
#7172 = PLANE ( 'NONE',  #1337 ) ;
#7173 = EDGE_LOOP ( 'NONE', ( #11564, #3286, #8573, #13760 ) ) ;
#7174 = LINE ( 'NONE', #8943, #3597 ) ;
#7175 = AXIS2_PLACEMENT_3D ( 'NONE', #5253, #13589, #15158 ) ;
#7176 = APPLICATION_CONTEXT ( 'automotive_design' ) ;
#7177 = FACE_OUTER_BOUND ( 'NONE', #17570, .T. ) ;
#7178 = CARTESIAN_POINT ( 'NONE',  ( 10.09176930091618196, 9.223890154941049246, 47.65417223256151402 ) ) ;
#7179 = ORIENTED_EDGE ( 'NONE', *, *, #16889, .T. ) ;
#7180 = CARTESIAN_POINT ( 'NONE',  ( -70.71978124295696944, -111.0842361345572158, 18.23991632971911869 ) ) ;
#7181 = DIRECTION ( 'NONE',  ( 0.000000000000000000, 0.000000000000000000, -1.000000000000000000 ) ) ;
#7182 = DIRECTION ( 'NONE',  ( 1.156482317317869999E-16, 0.000000000000000000, 1.000000000000000000 ) ) ;
#7183 = LINE ( 'NONE', #17003, #13160 ) ;
#7184 = ORIENTED_EDGE ( 'NONE', *, *, #16915, .T. ) ;
#7185 = VECTOR ( 'NONE', #9848, 1000.000000000000000 ) ;
#7186 = VERTEX_POINT ( 'NONE', #4856 ) ;
#7187 = EDGE_CURVE ( 'NONE', #17297, #794, #4495, .T. ) ;
#7188 = CIRCLE ( 'NONE', #17619, 12.50000000000001066 ) ;
#7189 = CARTESIAN_POINT ( 'NONE',  ( -64.58002265617299997, 84.22855780814606419, -167.1454815528550739 ) ) ;
#7190 = ORIENTED_EDGE ( 'NONE', *, *, #2184, .F. ) ;
#7191 = SHAPE_REPRESENTATION_RELATIONSHIP ( 'NONE' , 'NONE' ,  #1677, #5898 ) ;
#7192 = CARTESIAN_POINT ( 'NONE',  ( -66.42454906961714300, 112.0712930187555827, -27.77368723278591744 ) ) ;
#7193 = FACE_OUTER_BOUND ( 'NONE', #9419, .T. ) ;
#7194 = DIRECTION ( 'NONE',  ( 1.000000000000000000, 0.000000000000000000, 0.000000000000000000 ) ) ;
#7195 = ORIENTED_EDGE ( 'NONE', *, *, #1601, .F. ) ;
#7196 = VECTOR ( 'NONE', #15393, 1000.000000000000000 ) ;
#7197 = PLANE ( 'NONE',  #14651 ) ;
#7198 = DIRECTION ( 'NONE',  ( -1.000000000000000000, 1.218656359355352799E-14, 1.692578276882434470E-16 ) ) ;
#7199 = CARTESIAN_POINT ( 'NONE',  ( -76.06514409945376087, 73.26749283226919829, 97.49999999999998579 ) ) ;
#7200 = CARTESIAN_POINT ( 'NONE',  ( 4.699999999999995737, 3.752776749732559924, -6.500000000000061284 ) ) ;
#7201 = VERTEX_POINT ( 'NONE', #7757 ) ;
#7203 = EDGE_CURVE ( 'NONE', #16062, #8476, #1255, .T. ) ;
#7202 = AXIS2_PLACEMENT_3D ( 'NONE', #11777, #17472, #10455 ) ;
#7204 = CARTESIAN_POINT ( 'NONE',  ( -68.99615306438110451, 14.57638228813026338, -15.00000000000001421 ) ) ;
#7205 = CIRCLE ( 'NONE', #16134, 4.000000000000024869 ) ;
#7206 = CARTESIAN_POINT ( 'NONE',  ( -107.5676225674731654, 57.88796029049330372, 26.35917033480641436 ) ) ;
#7207 = ORIENTED_EDGE ( 'NONE', *, *, #7035, .T. ) ;
#7208 = CARTESIAN_POINT ( 'NONE',  ( 94.09522336508815954, 84.22855780814606419, 62.50000000000001421 ) ) ;
#7209 = CARTESIAN_POINT ( 'NONE',  ( 44.74549999999999272, 2.220446049250313081E-16, 4.000000000000024869 ) ) ;
#7210 = VERTEX_POINT ( 'NONE', #10208 ) ;
#7211 = ORIENTED_EDGE ( 'NONE', *, *, #232, .F. ) ;
#7212 = ADVANCED_FACE ( 'NONE', ( #10306 ), #14515, .T. ) ;
#7213 = ADVANCED_FACE ( 'NONE', ( #1693 ), #1877, .F. ) ;
#7214 = ADVANCED_FACE ( 'NONE', ( #6158 ), #14595, .F. ) ;
#7215 = AXIS2_PLACEMENT_3D ( 'NONE', #9485, #9871, #18108 ) ;
#7216 = VECTOR ( 'NONE', #2664, 1000.000000000000000 ) ;
#7217 = DIRECTION ( 'NONE',  ( -0.000000000000000000, -0.000000000000000000, -1.000000000000000000 ) ) ;
#7218 = LINE ( 'NONE', #14329, #10851 ) ;
#7219 = DIRECTION ( 'NONE',  ( -1.000000000000000000, -1.119176436114069332E-16, 0.000000000000000000 ) ) ;
#7220 = DIRECTION ( 'NONE',  ( -1.000000000000000000, 0.000000000000000000, 0.000000000000000000 ) ) ;
#7221 = CARTESIAN_POINT ( 'NONE',  ( -68.99615306438073503, 108.8241617881302261, 15.00000000000006928 ) ) ;
#7222 = ORIENTED_EDGE ( 'NONE', *, *, #13285, .F. ) ;
#7223 = EDGE_CURVE ( 'NONE', #1925, #18214, #5801, .T. ) ;
#7224 = CARTESIAN_POINT ( 'NONE',  ( -56.41614838398844256, 95.01461175692088545, -167.1454815528550739 ) ) ;
#7225 = VERTEX_POINT ( 'NONE', #11120 ) ;
#7226 = VECTOR ( 'NONE', #1243, 1000.000000000000000 ) ;
#7227 = CARTESIAN_POINT ( 'NONE',  ( -61.60537251683745552, 75.03273214436880778, -15.00000000000001421 ) ) ;
#7228 = ADVANCED_FACE ( 'NONE', ( #5394 ), #6806, .T. ) ;
#7229 = EDGE_CURVE ( 'NONE', #13353, #15968, #12439, .T. ) ;
#7230 = DIRECTION ( 'NONE',  ( 0.000000000000000000, 0.000000000000000000, 1.000000000000000000 ) ) ;
#7231 = ORIENTED_EDGE ( 'NONE', *, *, #7120, .T. ) ;
#7232 = AXIS2_PLACEMENT_3D ( 'NONE', #12567, #2452, #9660 ) ;
#7233 = VECTOR ( 'NONE', #17569, 1000.000000000000000 ) ;
#7234 = DIRECTION ( 'NONE',  ( 1.000000000000000000, 0.000000000000000000, 0.000000000000000000 ) ) ;
#7235 = EDGE_LOOP ( 'NONE', ( #12002, #14232, #10575, #9047, #7096, #1172, #13328 ) ) ;
#7236 = EDGE_CURVE ( 'NONE', #6571, #7186, #9606, .T. ) ;
#7237 = EDGE_CURVE ( 'NONE', #538, #14988, #7530, .T. ) ;
#7238 = ORIENTED_EDGE ( 'NONE', *, *, #8238, .F. ) ;
#7239 = DIRECTION ( 'NONE',  ( 1.000000000000000000, 0.000000000000000000, 3.771137991253928573E-16 ) ) ;
#7240 = DIRECTION ( 'NONE',  ( 0.9396926207859084279, 0.3420201433256686574, -1.086737899652989892E-16 ) ) ;
#7241 = DIRECTION ( 'NONE',  ( -1.000000000000000000, -0.000000000000000000, -0.000000000000000000 ) ) ;
#7242 = ORIENTED_EDGE ( 'NONE', *, *, #12576, .F. ) ;
#7243 = VECTOR ( 'NONE', #6510, 1000.000000000000000 ) ;
#7244 = AXIS2_PLACEMENT_3D ( 'NONE', #15982, #8882, #14575 ) ;
#7245 = CARTESIAN_POINT ( 'NONE',  ( -26.78696867915027724, -93.09900487505512956, 6.628864488196846594 ) ) ;
#7246 = ORIENTED_EDGE ( 'NONE', *, *, #8810, .F. ) ;
#7247 = DIRECTION ( 'NONE',  ( -3.223492141267075737E-15, 0.000000000000000000, 1.000000000000000000 ) ) ;
#7248 = CARTESIAN_POINT ( 'NONE',  ( -94.45685920050698314, -47.21335801510345220, 15.00000000000006928 ) ) ;
#7249 = LINE ( 'NONE', #17514, #6036 ) ;
#7250 = VERTEX_POINT ( 'NONE', #4186 ) ;
#7251 = EDGE_CURVE ( 'NONE', #2786, #2549, #2693, .T. ) ;
#7252 = CARTESIAN_POINT ( 'NONE',  ( 0.000000000000000000, -96.08423613455721579, -5.654315315325675328 ) ) ;
#7253 = ORIENTED_EDGE ( 'NONE', *, *, #15718, .T. ) ;
#7254 = ORIENTED_EDGE ( 'NONE', *, *, #13983, .T. ) ;
#7255 = AXIS2_PLACEMENT_3D ( 'NONE', #7788, #2171, #2266 ) ;
#7256 = ORIENTED_EDGE ( 'NONE', *, *, #3112, .T. ) ;
#7257 = LINE ( 'NONE', #7427, #6693 ) ;
#7258 = LINE ( 'NONE', #160, #13258 ) ;
#7259 = DIRECTION ( 'NONE',  ( -1.000000000000000000, 0.000000000000000000, 0.000000000000000000 ) ) ;
#7260 = VECTOR ( 'NONE', #11591, 1000.000000000000000 ) ;
#7261 = VERTEX_POINT ( 'NONE', #18131 ) ;
#7262 = CARTESIAN_POINT ( 'NONE',  ( -46.71322837820016360, 91.21279551874765446, -15.00000000000001421 ) ) ;
#7263 = CARTESIAN_POINT ( 'NONE',  ( -79.12361985383350316, 84.22855780814606419, -47.50000000000000000 ) ) ;
#7264 = CARTESIAN_POINT ( 'NONE',  ( -68.99615306438094819, 52.27549408813023746, 15.00000000000006928 ) ) ;
#7265 = CARTESIAN_POINT ( 'NONE',  ( -57.08002265617300708, 84.22855780814606419, 15.00000000000006928 ) ) ;
#7266 = ORIENTED_EDGE ( 'NONE', *, *, #4038, .F. ) ;
#7267 = CARTESIAN_POINT ( 'NONE',  ( -57.35243698450333483, 71.73152654333280509, 15.00000000000006928 ) ) ;
#7268 = VECTOR ( 'NONE', #3631, 1000.000000000000000 ) ;
#7269 = CIRCLE ( 'NONE', #1590, 4.599999999999999645 ) ;
#7270 = AXIS2_PLACEMENT_3D ( 'NONE', #7105, #4198, #4297 ) ;
#7271 = CARTESIAN_POINT ( 'NONE',  ( -97.59262256747319952, 57.88796029049330372, -26.35917033480641436 ) ) ;
#7272 = DIRECTION ( 'NONE',  ( 0.000000000000000000, 0.000000000000000000, -1.000000000000000000 ) ) ;
#7273 = ORIENTED_EDGE ( 'NONE', *, *, #6778, .T. ) ;
#7274 = B_SPLINE_CURVE_WITH_KNOTS ( 'NONE', 3,
 ( #10307, #8633, #6075, #5980, #12946, #10388, #14337, #7588, #15825, #18, #5719, #7320, #1780, #1520, #208, #17139, #285, #13037, #4590, #11709 ),
 .UNSPECIFIED., .F., .F.,
 ( 4, 2, 2, 2, 2, 2, 2, 2, 2, 4 ),
 ( 0.000000000000000000, 0.001278592738658794990, 0.002557185477317589981, 0.003835778215976384971, 0.005114370954635179961, 0.006392963693293974084, 0.007671556431952769942, 0.008950149170611565799, 0.009589445539940970667, 0.01022874190927037553 ),
 .UNSPECIFIED. ) ;
#7275 = CARTESIAN_POINT ( 'NONE',  ( -68.99615306438077766, 118.2489397381302751, 15.00000000000006928 ) ) ;
#7276 = B_SPLINE_CURVE_WITH_KNOTS ( 'NONE', 3,
 ( #1340, #12842, #6, #4319, #7393, #8717, #17300, #15905 ),
 .UNSPECIFIED., .F., .F.,
 ( 4, 2, 2, 4 ),
 ( 0.003797433802554418120, 0.004743183970586237024, 0.005688934138618055927, 0.007580434474681694602 ),
 .UNSPECIFIED. ) ;
#7277 = VECTOR ( 'NONE', #17828, 1000.000000000000000 ) ;
#7278 = CARTESIAN_POINT ( 'NONE',  ( -71.24615306438096241, 60.26648315456373695, -15.00000000000001421 ) ) ;
#7279 = ORIENTED_EDGE ( 'NONE', *, *, #12315, .F. ) ;
#7280 = ORIENTED_EDGE ( 'NONE', *, *, #5023, .T. ) ;
#7281 = AXIS2_PLACEMENT_3D ( 'NONE', #8028, #5316, #12164 ) ;
#7282 = VECTOR ( 'NONE', #3599, 1000.000000000000000 ) ;
#7284 = EDGE_CURVE ( 'NONE', #8311, #5735, #1201, .T. ) ;
#7283 = LINE ( 'NONE', #3064, #15021 ) ;
#7285 = DIRECTION ( 'NONE',  ( 0.000000000000000000, 0.000000000000000000, -1.000000000000000000 ) ) ;
#7286 = LINE ( 'NONE', #10447, #7260 ) ;
#7287 = CARTESIAN_POINT ( 'NONE',  ( -69.26154997389616597, 110.9670925573097833, -22.35917033480641791 ) ) ;
#7288 = EDGE_LOOP ( 'NONE', ( #8021, #8828, #11090, #756 ) ) ;
#7289 = CLOSED_SHELL ( 'NONE', ( #17953, #3114, #16922, #8850, #10766, #5368, #3258, #6769, #9973, #5325, #4034, #15212, #9051, #16013, #14239, #17492, #3908, #12391, #4435, #4023, #9498, #7131, #14831, #14301, #18448, #13053, #10287, #13152, #1342, #15465, #16678, #17062, #16199, #8325, #7445, #5929, #17815, #16962, #7214 ) ) ;
#7290 = DIRECTION ( 'NONE',  ( -0.000000000000000000, -0.000000000000000000, 1.000000000000000000 ) ) ;
#7291 = DIRECTION ( 'NONE',  ( 0.000000000000000000, 5.551115123125747573E-17, 1.000000000000000000 ) ) ;
#7292 = FACE_OUTER_BOUND ( 'NONE', #4790, .T. ) ;
#7293 = CARTESIAN_POINT ( 'NONE',  ( 0.000000000000000000, -4.857225732735059864E-14, 6.500000000000037303 ) ) ;
#7294 = ORIENTED_EDGE ( 'NONE', *, *, #16212, .F. ) ;
#7295 = CARTESIAN_POINT ( 'NONE',  ( -37.27435264852402241, 91.34252568597628397, 64.92569797180529179 ) ) ;
#7296 = AXIS2_PLACEMENT_3D ( 'NONE', #1007, #13718, #7927 ) ;
#7297 = AXIS2_PLACEMENT_3D ( 'NONE', #4134, #9839, #2444 ) ;
#7298 = LINE ( 'NONE', #10106, #9271 ) ;
#7299 = ORIENTED_EDGE ( 'NONE', *, *, #16354, .F. ) ;
#7300 = DIRECTION ( 'NONE',  ( -0.000000000000000000, -0.000000000000000000, -1.000000000000000000 ) ) ;
#7301 = DIRECTION ( 'NONE',  ( -5.204170427930409450E-16, 0.000000000000000000, 1.000000000000000000 ) ) ;
#7302 = ORIENTED_EDGE ( 'NONE', *, *, #10534, .T. ) ;
#7303 = ORIENTED_EDGE ( 'NONE', *, *, #5351, .F. ) ;
#7304 = VECTOR ( 'NONE', #5571, 1000.000000000000000 ) ;
#7306 = EDGE_CURVE ( 'NONE', #7123, #1636, #16171, .T. ) ;
#7305 = ORIENTED_EDGE ( 'NONE', *, *, #8130, .F. ) ;
#7307 = AXIS2_PLACEMENT_3D ( 'NONE', #9198, #3484, #10687 ) ;
#7308 = AXIS2_PLACEMENT_3D ( 'NONE', #9304, #2365, #12409 ) ;
#7309 = AXIS2_PLACEMENT_3D ( 'NONE', #17388, #11699, #201 ) ;
#7310 = DIRECTION ( 'NONE',  ( -4.675871521838984962E-16, 1.000000000000000000, 0.000000000000000000 ) ) ;
#7311 = LINE ( 'NONE', #1687, #2793 ) ;
#7312 = CARTESIAN_POINT ( 'NONE',  ( 95.45835937779682467, 4.463510241361116170E-14, 3.000000000000000000 ) ) ;
#7313 = CARTESIAN_POINT ( 'NONE',  ( -68.99615306438089135, 86.21815738166266385, -15.00000000000001421 ) ) ;
#7314 = DIRECTION ( 'NONE',  ( -0.9396926207859158664, 0.3420201433256481738, 0.000000000000000000 ) ) ;
#7315 = ORIENTED_EDGE ( 'NONE', *, *, #903, .T. ) ;
#7316 = VECTOR ( 'NONE', #4623, 1000.000000000000000 ) ;
#7317 = DIRECTION ( 'NONE',  ( -5.204170427930409450E-16, 0.000000000000000000, 1.000000000000000000 ) ) ;
#7318 = ORIENTED_EDGE ( 'NONE', *, *, #12240, .T. ) ;
#7319 = EDGE_CURVE ( 'NONE', #14830, #7990, #10933, .T. ) ;
#7320 = CARTESIAN_POINT ( 'NONE',  ( -79.28150129717909067, -91.53393135689866256, 41.62626982970570566 ) ) ;
#7321 = CARTESIAN_POINT ( 'NONE',  ( -67.77554565888843285, 85.77305660501664875, -15.00000000000001421 ) ) ;
#7322 = VERTEX_POINT ( 'NONE', #2606 ) ;
#7323 = AXIS2_PLACEMENT_3D ( 'NONE', #16708, #1395, #2890 ) ;
#7324 = PLANE ( 'NONE',  #2249 ) ;
#7325 = CARTESIAN_POINT ( 'NONE',  ( -52.17393402261416213, 74.59995546124159205, 15.00000000000006928 ) ) ;
#7327 = ORIENTED_EDGE ( 'NONE', *, *, #8605, .T. ) ;
#7326 = AXIS2_PLACEMENT_3D ( 'NONE', #16325, #5004, #2116 ) ;
#7328 = ADVANCED_FACE ( 'NONE', ( #3811 ), #9513, .T. ) ;
#7329 = ADVANCED_FACE ( 'NONE', ( #2397 ), #6900, .T. ) ;
#7330 = ORIENTED_EDGE ( 'NONE', *, *, #2492, .T. ) ;
#7331 = ADVANCED_FACE ( 'NONE', ( #8863 ), #11752, .T. ) ;
#7332 = LINE ( 'NONE', #14605, #4039 ) ;
#7333 = CARTESIAN_POINT ( 'NONE',  ( -102.5926225674731569, 65.58224449241410525, -20.00000000000000355 ) ) ;
#7334 = CARTESIAN_POINT ( 'NONE',  ( -68.99615306438106188, 36.56753083813027416, -167.1454815528550739 ) ) ;
#7335 = VECTOR ( 'NONE', #2331, 1000.000000000000000 ) ;
#7336 = ORIENTED_EDGE ( 'NONE', *, *, #13609, .F. ) ;
#7337 = AXIS2_PLACEMENT_3D ( 'NONE', #13642, #6425, #13926 ) ;
#7338 = CIRCLE ( 'NONE', #6746, 10.24900000000000055 ) ;
#7339 = ORIENTED_EDGE ( 'NONE', *, *, #15713, .F. ) ;
#7340 = EDGE_CURVE ( 'NONE', #12366, #15968, #14557, .T. ) ;
#7341 = CARTESIAN_POINT ( 'NONE',  ( -71.24615306438109030, 24.82009326522924297, -15.00000000000001421 ) ) ;
#7342 = CYLINDRICAL_SURFACE ( 'NONE', #13501, 3.999999999999989786 ) ;
#7343 = DIRECTION ( 'NONE',  ( 1.156482317317869999E-16, 0.000000000000000000, 1.000000000000000000 ) ) ;
#7344 = EDGE_CURVE ( 'NONE', #7683, #857, #1276, .T. ) ;
#7345 = CARTESIAN_POINT ( 'NONE',  ( -68.99615306438083451, 98.78452798166264870, -15.00000000000001421 ) ) ;
#7346 = EDGE_CURVE ( 'NONE', #5470, #2933, #1470, .T. ) ;
#7347 = ORIENTED_EDGE ( 'NONE', *, *, #9355, .T. ) ;
#7348 = CARTESIAN_POINT ( 'NONE',  ( -107.5926225674732137, 117.8748711238780373, 35.00000000000000000 ) ) ;
#7349 = VERTEX_POINT ( 'NONE', #11578 ) ;
#7350 = ADVANCED_FACE ( 'NONE', ( #14375 ), #328, .T. ) ;
#7351 = VERTEX_POINT ( 'NONE', #5935 ) ;
#7352 = EDGE_CURVE ( 'NONE', #5195, #6193, #15705, .T. ) ;
#7353 = VECTOR ( 'NONE', #11518, 1000.000000000000000 ) ;
#7354 = VERTEX_POINT ( 'NONE', #8772 ) ;
#7355 = EDGE_CURVE ( 'NONE', #17247, #3974, #12926, .T. ) ;
#7356 = PRESENTATION_STYLE_ASSIGNMENT (( #16110 ) ) ;
#7357 = EDGE_CURVE ( 'NONE', #16195, #2018, #958, .T. ) ;
#7358 = LINE ( 'NONE', #5923, #5777 ) ;
#7359 = VERTEX_POINT ( 'NONE', #3152 ) ;
#7360 = LINE ( 'NONE', #12797, #11638 ) ;
#7361 = LINE ( 'NONE', #11489, #2964 ) ;
#7362 = DIRECTION ( 'NONE',  ( 0.000000000000000000, 1.000000000000000000, 0.000000000000000000 ) ) ;
#7363 = CARTESIAN_POINT ( 'NONE',  ( 0.000000000000000000, 3.608224830031758263E-16, 6.500000000000039968 ) ) ;
#7364 = EDGE_LOOP ( 'NONE', ( #5260, #6059, #13655, #5043 ) ) ;
#7365 = DIRECTION ( 'NONE',  ( 0.3420201433256649937, -0.9396926207859097602, 0.000000000000000000 ) ) ;
#7366 = CARTESIAN_POINT ( 'NONE',  ( -71.24615306438076345, 122.2094654152292037, 15.00000000000006928 ) ) ;
#7367 = DIRECTION ( 'NONE',  ( 1.000000000000000000, 2.062304371594500494E-16, -2.775557561562890858E-16 ) ) ;
#7368 = ORIENTED_EDGE ( 'NONE', *, *, #4667, .T. ) ;
#7369 = DIRECTION ( 'NONE',  ( 0.000000000000000000, -0.000000000000000000, -1.000000000000000000 ) ) ;
#7370 = CARTESIAN_POINT ( 'NONE',  ( -171.0109138863553824, 84.22855780814606419, 62.50000000000001421 ) ) ;
#7371 = ORIENTED_EDGE ( 'NONE', *, *, #10526, .T. ) ;
#7372 = ORIENTED_EDGE ( 'NONE', *, *, #18318, .T. ) ;
#7373 = CYLINDRICAL_SURFACE ( 'NONE', #2485, 4.599999999999992539 ) ;
#7374 = CARTESIAN_POINT ( 'NONE',  ( 0.000000000000000000, 0.000000000000000000, 0.000000000000000000 ) ) ;
#7375 = CARTESIAN_POINT ( 'NONE',  ( -71.24615306438089135, 81.36876096522922808, -15.00000000000001421 ) ) ;
#7376 = DIRECTION ( 'NONE',  ( 0.000000000000000000, 0.000000000000000000, 1.000000000000000000 ) ) ;
#7377 = ORIENTED_EDGE ( 'NONE', *, *, #9740, .T. ) ;
#7378 = FACE_OUTER_BOUND ( 'NONE', #8658, .T. ) ;
#7379 = DIRECTION ( 'NONE',  ( -5.204170427930409450E-16, 0.000000000000000000, 1.000000000000000000 ) ) ;
#7380 = DIRECTION ( 'NONE',  ( -0.000000000000000000, -0.000000000000000000, -1.000000000000000000 ) ) ;
#7381 = CARTESIAN_POINT ( 'NONE',  ( 0.4053525175236455391, 3.145852061456137161, 6.499999999999982236 ) ) ;
#7382 = CARTESIAN_POINT ( 'NONE',  ( -37.34514748644593851, 91.53406102980444814, 60.78507314490369140 ) ) ;
#7383 = CARTESIAN_POINT ( 'NONE',  ( -71.24615306438086293, 100.2183168652291982, -167.1454815528550739 ) ) ;
#7384 = EDGE_LOOP ( 'NONE', ( #2601, #1212, #8871, #14257 ) ) ;
#7385 = PRODUCT_DEFINITION ( 'UNKNOWN', '', #10862, #15066 ) ;
#7386 = DIRECTION ( 'NONE',  ( 1.000000000000000000, 0.000000000000000000, 0.000000000000000000 ) ) ;
#7387 = DIRECTION ( 'NONE',  ( 0.000000000000000000, 0.000000000000000000, -1.000000000000000000 ) ) ;
#7388 = ORIENTED_EDGE ( 'NONE', *, *, #9753, .T. ) ;
#7389 = ORIENTED_EDGE ( 'NONE', *, *, #10075, .F. ) ;
#7390 = ADVANCED_FACE ( 'NONE', ( #11399 ), #5768, .T. ) ;
#7391 = ORIENTED_EDGE ( 'NONE', *, *, #7082, .F. ) ;
#7392 = LINE ( 'NONE', #3261, #12709 ) ;
#7393 = CARTESIAN_POINT ( 'NONE',  ( 0.1061556211656023985, -4.836380039389555741, 4.623144047065584239 ) ) ;
#7394 = DIRECTION ( 'NONE',  ( -5.204170427930409450E-16, 0.000000000000000000, 1.000000000000000000 ) ) ;
#7395 = DIRECTION ( 'NONE',  ( 1.000000000000000000, 2.062304371594500740E-16, -0.000000000000000000 ) ) ;
#7396 = CARTESIAN_POINT ( 'NONE',  ( -71.24615306438101925, 44.55851990456372391, -15.00000000000001421 ) ) ;
#7397 = ORIENTED_EDGE ( 'NONE', *, *, #18075, .T. ) ;
#7398 = CARTESIAN_POINT ( 'NONE',  ( -68.99615306438100504, 45.37745293166267402, 15.00000000000006928 ) ) ;
#7399 = DIRECTION ( 'NONE',  ( 0.3420201433256520596, -0.9396926207859145341, 0.000000000000000000 ) ) ;
#7400 = CARTESIAN_POINT ( 'NONE',  ( -71.24615306438107609, 25.70896400456377506, -15.00000000000001421 ) ) ;
#7401 = ORIENTED_EDGE ( 'NONE', *, *, #4891, .T. ) ;
#7402 = DIRECTION ( 'NONE',  ( -1.000000000000000000, 0.000000000000000000, 0.000000000000000000 ) ) ;
#7403 = CARTESIAN_POINT ( 'NONE',  ( -109.8630080638463511, -91.08423613455720158, -10.52500441287596011 ) ) ;
#7404 = VERTEX_POINT ( 'NONE', #7094 ) ;
#7405 = ORIENTED_EDGE ( 'NONE', *, *, #1727, .F. ) ;
#7406 = EDGE_CURVE ( 'NONE', #10257, #15993, #2887, .T. ) ;
#7407 = CARTESIAN_POINT ( 'NONE',  ( -97.59262256747319952, 106.8071537307723133, 25.00000000000000000 ) ) ;
#7408 = LINE ( 'NONE', #12962, #13275 ) ;
#7409 = LINE ( 'NONE', #11625, #17103 ) ;
#7410 = ORIENTED_EDGE ( 'NONE', *, *, #14416, .F. ) ;
#7411 = ORIENTED_EDGE ( 'NONE', *, *, #10304, .T. ) ;
#7412 = CIRCLE ( 'NONE', #13386, 29.36884788726140627 ) ;
#7413 = DIRECTION ( 'NONE',  ( -0.9240607556975078962, -0.3822456275482439825, -1.060944741915880422E-15 ) ) ;
#7414 = CARTESIAN_POINT ( 'NONE',  ( 0.2573354458088682462, -6.889406814520657285, 1.067197363239251295 ) ) ;
#7415 = CARTESIAN_POINT ( 'NONE',  ( -55.20348911625212907, 74.15281352429526862, -15.00000000000001421 ) ) ;
#7416 = DIRECTION ( 'NONE',  ( 0.000000000000000000, 0.000000000000000000, -1.000000000000000000 ) ) ;
#7417 = ORIENTED_EDGE ( 'NONE', *, *, #10999, .F. ) ;
#7418 = ADVANCED_FACE ( 'NONE', ( #10349 ), #1735, .T. ) ;
#7419 = DIRECTION ( 'NONE',  ( 1.000000000000000000, 0.000000000000000000, 0.000000000000000000 ) ) ;
#7420 = EDGE_LOOP ( 'NONE', ( #17630, #16514, #6005, #16324 ) ) ;
#7421 = EDGE_CURVE ( 'NONE', #8426, #18002, #12803, .T. ) ;
#7422 = ORIENTED_EDGE ( 'NONE', *, *, #8952, .F. ) ;
#7423 = AXIS2_PLACEMENT_3D ( 'NONE', #15351, #8330, #14045 ) ;
#7424 = ORIENTED_EDGE ( 'NONE', *, *, #12727, .T. ) ;
#7425 = EDGE_CURVE ( 'NONE', #7647, #12706, #9021, .T. ) ;
#7426 = ADVANCED_FACE ( 'NONE', ( #7177 ), #10159, .T. ) ;
#7427 = CARTESIAN_POINT ( 'NONE',  ( -71.24615306438083451, 97.07672421522921979, 15.00000000000006928 ) ) ;
#7428 = LINE ( 'NONE', #11484, #11175 ) ;
#7429 = CARTESIAN_POINT ( 'NONE',  ( 0.000000000000000000, -111.0842361345572158, 3.000000000000000000 ) ) ;
#7430 = VERTEX_POINT ( 'NONE', #4373 ) ;
#7431 = CARTESIAN_POINT ( 'NONE',  ( -48.65098454476478196, 77.46608744949921288, 15.00000000000006928 ) ) ;
#7432 = CARTESIAN_POINT ( 'NONE',  ( -67.12361985383350316, 84.22855780814606419, -61.50000000000001421 ) ) ;
#7433 = LINE ( 'NONE', #11745, #935 ) ;
#7434 = CARTESIAN_POINT ( 'NONE',  ( -66.63376473465912397, -19.34983604512935429, 3.000000000000000000 ) ) ;
#7435 = ORIENTED_EDGE ( 'NONE', *, *, #4242, .T. ) ;
#7436 = EDGE_CURVE ( 'NONE', #6896, #13777, #15864, .T. ) ;
#7437 = LINE ( 'NONE', #13246, #13468 ) ;
#7439 = ADVANCED_FACE ( 'NONE', ( #3407 ), #17812, .T. ) ;
#7438 = AXIS2_PLACEMENT_3D ( 'NONE', #6015, #8938, #3047 ) ;
#7440 = DIRECTION ( 'NONE',  ( 0.000000000000000000, 1.734723475976811433E-15, 1.000000000000000000 ) ) ;
#7441 = CARTESIAN_POINT ( 'NONE',  ( -57.08002265617300708, 84.22855780814606419, 15.00000000000006928 ) ) ;
#7442 = ORIENTED_EDGE ( 'NONE', *, *, #11343, .F. ) ;
#7443 = EDGE_CURVE ( 'NONE', #4219, #2450, #9322, .T. ) ;
#7444 = PLANE ( 'NONE',  #11808 ) ;
#7445 = ADVANCED_FACE ( 'NONE', ( #607 ), #13338, .F. ) ;
#7446 = FACE_OUTER_BOUND ( 'NONE', #12810, .T. ) ;
#7447 = ORIENTED_EDGE ( 'NONE', *, *, #8710, .F. ) ;
#7448 = ORIENTED_EDGE ( 'NONE', *, *, #15108, .T. ) ;
#7449 = EDGE_CURVE ( 'NONE', #7663, #13644, #16314, .T. ) ;
#7450 = ORIENTED_EDGE ( 'NONE', *, *, #17243, .F. ) ;
#7451 = CIRCLE ( 'NONE', #882, 180.8515291679561585 ) ;
#7452 = CARTESIAN_POINT ( 'NONE',  ( -71.24615306438091977, 75.08557566522922855, -15.00000000000001421 ) ) ;
#7453 = ORIENTED_EDGE ( 'NONE', *, *, #17392, .T. ) ;
#7454 = VECTOR ( 'NONE', #14055, 1000.000000000000000 ) ;
#7455 = DIRECTION ( 'NONE',  ( 0.000000000000000000, -0.06926051163264763944, 0.9975986074210329013 ) ) ;
#7456 = LINE ( 'NONE', #13176, #982 ) ;
#7457 = DIRECTION ( 'NONE',  ( 0.000000000000000000, 0.000000000000000000, 1.000000000000000000 ) ) ;
#7458 = EDGE_LOOP ( 'NONE', ( #9200, #10439, #13484, #7735 ) ) ;
#7459 = ADVANCED_BREP_SHAPE_REPRESENTATION ( '', ( #12831, #16217 ), #2819 ) ;
#7460 = CARTESIAN_POINT ( 'NONE',  ( -57.08002265617300708, 84.22855780814606419, -61.50000000000000000 ) ) ;
#7461 = LINE ( 'NONE', #13445, #13317 ) ;
#7462 = DIRECTION ( 'NONE',  ( -1.000000000000000000, 0.000000000000000000, 0.000000000000000000 ) ) ;
#7463 = DIRECTION ( 'NONE',  ( -1.000000000000000000, -0.000000000000000000, -0.000000000000000000 ) ) ;
#7464 = CARTESIAN_POINT ( 'NONE',  ( -36.53593263535576341, 88.80498052294456102, 56.53818285498137186 ) ) ;
#7465 = CARTESIAN_POINT ( 'NONE',  ( -71.24615306438109030, 27.96168591522921076, -15.00000000000001421 ) ) ;
#7466 = CIRCLE ( 'NONE', #17907, 10.38004356723770627 ) ;
#7467 = EDGE_LOOP ( 'NONE', ( #213, #10589, #6918, #500 ) ) ;
#7468 = CARTESIAN_POINT ( 'NONE',  ( -67.42374588395286139, 61.35112309735787761, 25.00000000000000355 ) ) ;
#7469 = VECTOR ( 'NONE', #8720, 1000.000000000000000 ) ;
#7470 = LINE ( 'NONE', #13189, #911 ) ;
#7471 = ORIENTED_EDGE ( 'NONE', *, *, #7664, .T. ) ;
#7472 = VECTOR ( 'NONE', #639, 1000.000000000000000 ) ;
#7473 = ORIENTED_EDGE ( 'NONE', *, *, #8822, .T. ) ;
#7474 = COLOUR_RGB ( '',0.7921568627450980005, 0.8196078431372548767, 0.9333333333333333481 ) ;
#7475 = EDGE_LOOP ( 'NONE', ( #5549, #3830, #2780, #5372 ) ) ;
#7476 = CARTESIAN_POINT ( 'NONE',  ( -57.08002265617300708, 84.22855780814606419, 15.00000000000006928 ) ) ;
#7477 = DIRECTION ( 'NONE',  ( 1.156482317317869999E-16, 0.000000000000000000, 1.000000000000000000 ) ) ;
#7478 = VECTOR ( 'NONE', #8326, 1000.000000000000000 ) ;
#7479 = CARTESIAN_POINT ( 'NONE',  ( 15.23320273812466574, -111.0842361345572158, -57.00000000000000000 ) ) ;
#7480 = FACE_OUTER_BOUND ( 'NONE', #13878, .T. ) ;
#7481 = PRODUCT_DEFINITION ( 'UNKNOWN', '', #9987, #3840 ) ;
#7482 = FACE_OUTER_BOUND ( 'NONE', #15747, .T. ) ;
#7483 = EDGE_CURVE ( 'NONE', #4400, #2613, #10706, .T. ) ;
#7484 = CARTESIAN_POINT ( 'NONE',  ( -57.08002265617300708, 84.22855780814606419, -15.00000000000001421 ) ) ;
#7485 = PLANE ( 'NONE',  #17369 ) ;
#7486 = AXIS2_PLACEMENT_3D ( 'NONE', #12156, #13650, #12058 ) ;
#7487 = ORIENTED_EDGE ( 'NONE', *, *, #1148, .F. ) ;
#7488 = DIRECTION ( 'NONE',  ( -1.000000000000000000, -2.062304371594500494E-16, 2.775557561562890858E-16 ) ) ;
#7489 = LINE ( 'NONE', #13206, #8479 ) ;
#7490 = DIRECTION ( 'NONE',  ( 1.000000000000000000, 0.000000000000000000, 0.000000000000000000 ) ) ;
#7491 = ORIENTED_EDGE ( 'NONE', *, *, #9376, .F. ) ;
#7492 = VECTOR ( 'NONE', #12970, 1000.000000000000000 ) ;
#7493 = LINE ( 'NONE', #1697, #4340 ) ;
#7494 = CARTESIAN_POINT ( 'NONE',  ( -71.24615306438103346, 47.70011255456374499, -15.00000000000001421 ) ) ;
#7495 = ORIENTED_EDGE ( 'NONE', *, *, #7904, .F. ) ;
#7496 = VECTOR ( 'NONE', #4372, 1000.000000000000000 ) ;
#7497 = AXIS2_PLACEMENT_3D ( 'NONE', #14468, #16037, #14553 ) ;
#7498 = ORIENTED_EDGE ( 'NONE', *, *, #2640, .F. ) ;
#7499 = DIRECTION ( 'NONE',  ( -1.000000000000000000, 0.000000000000000000, 0.000000000000000000 ) ) ;
#7500 = FACE_OUTER_BOUND ( 'NONE', #14200, .T. ) ;
#7501 = EDGE_CURVE ( 'NONE', #11410, #10310, #12207, .T. ) ;
#7502 = LINE ( 'NONE', #8911, #12323 ) ;
#7503 = VERTEX_POINT ( 'NONE', #13423 ) ;
#7504 = CIRCLE ( 'NONE', #6008, 4.599999999999999645 ) ;
#7505 = VERTEX_POINT ( 'NONE', #9308 ) ;
#7506 = CARTESIAN_POINT ( 'NONE',  ( -92.59262256747321373, 110.5691553257988460, 26.35917033480641436 ) ) ;
#7507 = DIRECTION ( 'NONE',  ( 0.000000000000000000, 1.000000000000000000, 0.000000000000000000 ) ) ;
#7508 = DIRECTION ( 'NONE',  ( 1.000000000000000000, 2.062304371594500740E-16, -0.000000000000000000 ) ) ;
#7509 = DIRECTION ( 'NONE',  ( 1.156482317317869999E-16, 0.000000000000000000, 1.000000000000000000 ) ) ;
#7510 = AXIS2_PLACEMENT_3D ( 'NONE', #2562, #8262, #15730 ) ;
#7511 = VECTOR ( 'NONE', #2642, 1000.000000000000000 ) ;
#7512 = VERTEX_POINT ( 'NONE', #2198 ) ;
#7513 = CARTESIAN_POINT ( 'NONE',  ( -68.99615306438089135, 83.69142058813029905, 15.00000000000006928 ) ) ;
#7514 = ORIENTED_EDGE ( 'NONE', *, *, #17064, .F. ) ;
#7515 = DIRECTION ( 'NONE',  ( -2.062304371594500494E-16, 1.000000000000000000, -0.000000000000000000 ) ) ;
#7516 = ORIENTED_EDGE ( 'NONE', *, *, #6152, .F. ) ;
#7517 = VECTOR ( 'NONE', #9410, 1000.000000000000000 ) ;
#7518 = APPLICATION_CONTEXT ( 'automotive_design' ) ;
#7519 = VERTEX_POINT ( 'NONE', #9129 ) ;
#7520 = AXIS2_PLACEMENT_3D ( 'NONE', #13096, #9923, #11596 ) ;
#7521 = CARTESIAN_POINT ( 'NONE',  ( -208.2552686774341737, 84.22855780814606419, 62.50000000000001421 ) ) ;
#7522 = LINE ( 'NONE', #17252, #13866 ) ;
#7523 = CARTESIAN_POINT ( 'NONE',  ( -68.99615306438094819, 54.80223088166269463, -15.00000000000001421 ) ) ;
#7524 = ORIENTED_EDGE ( 'NONE', *, *, #17503, .T. ) ;
#7525 = EDGE_CURVE ( 'NONE', #17396, #16262, #7632, .T. ) ;
#7526 = DIRECTION ( 'NONE',  ( -0.000000000000000000, -1.000000000000000000, -0.000000000000000000 ) ) ;
#7527 = DIRECTION ( 'NONE',  ( -0.000000000000000000, -1.000000000000000000, 0.000000000000000000 ) ) ;
#7528 = CARTESIAN_POINT ( 'NONE',  ( 0.4042117618284869485, -3.141900367810146921, 6.499999999999983125 ) ) ;
#7529 = ORIENTED_EDGE ( 'NONE', *, *, #1497, .T. ) ;
#7530 = CIRCLE ( 'NONE', #3637, 4.599999999999999645 ) ;
#7531 = DIRECTION ( 'NONE',  ( 0.9396926207859097602, 0.3420201433256649937, 0.000000000000000000 ) ) ;
#7532 = DIRECTION ( 'NONE',  ( -1.000000000000000000, 0.000000000000000000, 0.000000000000000000 ) ) ;
#7533 = CARTESIAN_POINT ( 'NONE',  ( -107.5926225674732137, 117.8748711238780373, 35.00000000000000000 ) ) ;
#7534 = ORIENTED_EDGE ( 'NONE', *, *, #6512, .T. ) ;
#7535 = EDGE_CURVE ( 'NONE', #3299, #11538, #3328, .T. ) ;
#7536 = CIRCLE ( 'NONE', #12947, 6.500000000000039968 ) ;
#7537 = AXIS2_PLACEMENT_3D ( 'NONE', #13749, #8134, #937 ) ;
#7538 = FACE_OUTER_BOUND ( 'NONE', #13663, .T. ) ;
#7539 = DIRECTION ( 'NONE',  ( 0.000000000000000000, 0.000000000000000000, 1.000000000000000000 ) ) ;
#7540 = ORIENTED_EDGE ( 'NONE', *, *, #11329, .T. ) ;
#7541 = ORIENTED_EDGE ( 'NONE', *, *, #15095, .F. ) ;
#7542 = VECTOR ( 'NONE', #13050, 1000.000000000000000 ) ;
#7543 = ADVANCED_FACE ( 'NONE', ( #10432 ), #6397, .T. ) ;
#7544 = VERTEX_POINT ( 'NONE', #4712 ) ;
#7545 = EDGE_CURVE ( 'NONE', #3187, #3490, #12313, .T. ) ;
#7546 = DIRECTION ( 'NONE',  ( 0.9915318908039647550, 0.000000000000000000, -0.1298634264091108326 ) ) ;
#7547 = EDGE_CURVE ( 'NONE', #3088, #17119, #4243, .T. ) ;
#7548 = VECTOR ( 'NONE', #10296, 1000.000000000000000 ) ;
#7549 = DIRECTION ( 'NONE',  ( 0.3420201433256686574, 0.9396926207859084279, -0.000000000000000000 ) ) ;
#7550 =( NAMED_UNIT ( * ) SI_UNIT ( $, .STERADIAN. ) SOLID_ANGLE_UNIT ( ) );
#7551 = LINE ( 'NONE', #14487, #17117 ) ;
#7552 = EDGE_CURVE ( 'NONE', #1261, #5560, #13249, .T. ) ;
#7553 = CARTESIAN_POINT ( 'NONE',  ( -68.99615306438111872, 10.81993378166265529, -167.1454815528550739 ) ) ;
#7554 = ORIENTED_EDGE ( 'NONE', *, *, #6459, .T. ) ;
#7555 = LINE ( 'NONE', #1754, #8987 ) ;
#7556 = CARTESIAN_POINT ( 'NONE',  ( -97.59262256747319952, 110.5691553257988460, 26.35917033480641436 ) ) ;
#7557 = CARTESIAN_POINT ( 'NONE',  ( -107.5926225674731853, 110.5691553257988460, -22.33417033480641223 ) ) ;
#7558 = CYLINDRICAL_SURFACE ( 'NONE', #661, 12.58237727243326987 ) ;
#7559 = CARTESIAN_POINT ( 'NONE',  ( -36.07113975268146788, 85.46113186790836380, 69.90217987427729440 ) ) ;
#7560 = EDGE_CURVE ( 'NONE', #3332, #5163, #17724, .T. ) ;
#7561 = AXIS2_PLACEMENT_3D ( 'NONE', #16612, #3805, #14919 ) ;
#7562 = EDGE_CURVE ( 'NONE', #15190, #7061, #16124, .T. ) ;
#7563 = ADVANCED_FACE ( 'NONE', ( #9215 ), #3313, .T. ) ;
#7564 = DIRECTION ( 'NONE',  ( -0.9396926207859084279, 0.3420201433256686574, 1.086737899652989892E-16 ) ) ;
#7565 = ORIENTED_EDGE ( 'NONE', *, *, #17888, .F. ) ;
#7566 = ADVANCED_FACE ( 'NONE', ( #7711 ), #14905, .T. ) ;
#7567 = AXIS2_PLACEMENT_3D ( 'NONE', #4646, #8684, #258 ) ;
#7568 = DIRECTION ( 'NONE',  ( 1.000000000000000000, -0.000000000000000000, -0.000000000000000000 ) ) ;
#7569 = CIRCLE ( 'NONE', #1889, 4.599999999999992539 ) ;
#7570 = CARTESIAN_POINT ( 'NONE',  ( -36.17543036020666136, 81.80210967128934385, 55.39904201915711468 ) ) ;
#7571 = ORIENTED_EDGE ( 'NONE', *, *, #15339, .T. ) ;
#7572 = VERTEX_POINT ( 'NONE', #14993 ) ;
#7573 = ORIENTED_EDGE ( 'NONE', *, *, #16020, .F. ) ;
#7574 = EDGE_CURVE ( 'NONE', #2512, #4254, #2001, .T. ) ;
#7575 = DIRECTION ( 'NONE',  ( 1.000000000000000000, 0.000000000000000000, 5.077734830647309573E-16 ) ) ;
#7576 = CARTESIAN_POINT ( 'NONE',  ( -49.40461175531926585, 94.09456345901895702, -15.00000000000001421 ) ) ;
#7577 = ADVANCED_FACE ( 'NONE', ( #6573 ), #10896, .T. ) ;
#7578 = CARTESIAN_POINT ( 'NONE',  ( -46.10942163047475617, 78.23723799236688592, -167.1454815528550739 ) ) ;
#7579 = PLANE ( 'NONE',  #4947 ) ;
#7580 = PRODUCT_DEFINITION_FORMATION_WITH_SPECIFIED_SOURCE ( 'ANY', '', #2532, .NOT_KNOWN. ) ;
#7581 = DIRECTION ( 'NONE',  ( -0.004825104377941397994, -0.9999883591161159435, 0.000000000000000000 ) ) ;
#7582 = AXIS2_PLACEMENT_3D ( 'NONE', #18212, #6988, #1189 ) ;
#7583 = CARTESIAN_POINT ( 'NONE',  ( -68.99615306438080609, 108.2093059316626693, 15.00000000000006928 ) ) ;
#7584 = AXIS2_PLACEMENT_3D ( 'NONE', #3885, #2594, #9791 ) ;
#7585 = FACE_OUTER_BOUND ( 'NONE', #2032, .T. ) ;
#7586 = VERTEX_POINT ( 'NONE', #7801 ) ;
#7587 = CARTESIAN_POINT ( 'NONE',  ( -71.24615306438076345, 119.0678727652292253, -167.1454815528550739 ) ) ;
#7588 = CARTESIAN_POINT ( 'NONE',  ( -77.79035519103837260, -92.58100082067043957, 43.41642806912991404 ) ) ;
#7589 = CARTESIAN_POINT ( 'NONE',  ( -107.5926225674731711, 65.58224449241410525, 20.00000000000000355 ) ) ;
#7590 = VERTEX_POINT ( 'NONE', #13693 ) ;
#7591 = CARTESIAN_POINT ( 'NONE',  ( -70.27900850916093134, -47.21335801510345220, 15.00000000000008171 ) ) ;
#7592 = CARTESIAN_POINT ( 'NONE',  ( -71.24615306438074924, 110.5319655545637687, 15.00000000000006928 ) ) ;
#7593 = ORIENTED_EDGE ( 'NONE', *, *, #13622, .T. ) ;
#7594 = CIRCLE ( 'NONE', #17735, 170.8515291679562154 ) ;
#7595 = ORIENTED_EDGE ( 'NONE', *, *, #7806, .T. ) ;
#7596 = EDGE_CURVE ( 'NONE', #9962, #4700, #3051, .T. ) ;
#7597 = LINE ( 'NONE', #8737, #12092 ) ;
#7598 = CARTESIAN_POINT ( 'NONE',  ( -37.39761953508091352, 56.02837566180792805, -23.04006316738493609 ) ) ;
#7599 = CARTESIAN_POINT ( 'NONE',  ( -68.99615306438111872, 20.85956758813031797, -167.1454815528550739 ) ) ;
#7600 = AXIS2_PLACEMENT_3D ( 'NONE', #11892, #216, #5903 ) ;
#7601 = ORIENTED_EDGE ( 'NONE', *, *, #13483, .F. ) ;
#7602 = CARTESIAN_POINT ( 'NONE',  ( -42.53669312409158465, -91.08423613455721579, -5.654315315325675328 ) ) ;
#7603 = VERTEX_POINT ( 'NONE', #17992 ) ;
#7604 = VECTOR ( 'NONE', #2287, 1000.000000000000000 ) ;
#7605 = CARTESIAN_POINT ( 'NONE',  ( -92.59262256747321373, 117.8748711238780373, 35.00000000000000000 ) ) ;
#7606 = CARTESIAN_POINT ( 'NONE',  ( -57.08002265617300708, 84.22855780814606419, -167.1454815528550739 ) ) ;
#7607 = CARTESIAN_POINT ( 'NONE',  ( -127.5926225674731711, 61.64996188551982925, 25.00000000000000355 ) ) ;
#7608 = DIRECTION ( 'NONE',  ( 1.000000000000000000, 0.000000000000000000, 0.000000000000000000 ) ) ;
#7609 = VECTOR ( 'NONE', #8666, 1000.000000000000000 ) ;
#7610 = ORIENTED_EDGE ( 'NONE', *, *, #5133, .T. ) ;
#7611 = VECTOR ( 'NONE', #7666, 1000.000000000000000 ) ;
#7612 = PLANE ( 'NONE',  #1777 ) ;
#7613 = VERTEX_POINT ( 'NONE', #5179 ) ;
#7614 = DIRECTION ( 'NONE',  ( -0.000000000000000000, -0.000000000000000000, -1.000000000000000000 ) ) ;
#7615 = ORIENTED_EDGE ( 'NONE', *, *, #17064, .T. ) ;
#7616 = EDGE_CURVE ( 'NONE', #3179, #5307, #3580, .T. ) ;
#7617 = EDGE_LOOP ( 'NONE', ( #6708, #947, #3797, #1472, #9023, #13946, #12032, #4433, #4128, #7280, #6118, #5618, #8335, #1100, #4592, #351, #8145, #1185, #13385, #14939, #4267, #16284, #4817, #3351, #11170, #12652, #15630, #13453, #5373, #8774, #11627, #14891, #12193, #12159, #8199, #12813, #14686, #13667, #6056, #2517, #643, #1374, #605, #4141, #9049, #18118, #8725, #17559, #578, #17382, #4842, #14609, #6680, #785, #7529, #12789, #14990, #1767, #17414, #8190, #6186, #8315, #13557, #3848, #3238, #12476, #15530, #18397, #15280, #14060, #9979, #2105, #1147, #2039, #15499, #13621, #149, #7784, #10946, #18095, #2349, #9392, #17402, #17210, #1808, #14545, #7817, #9089, #10623, #1109, #5188, #11915, #16590, #9994, #1592 ) ) ;
#7618 = VERTEX_POINT ( 'NONE', #16208 ) ;
#7619 = AXIS2_PLACEMENT_3D ( 'NONE', #11000, #14001, #16685 ) ;
#7620 = EDGE_CURVE ( 'NONE', #1345, #6650, #2094, .T. ) ;
#7621 = CIRCLE ( 'NONE', #10916, 4.599999999999992539 ) ;
#7622 = CIRCLE ( 'NONE', #452, 29.36884788726140627 ) ;
#7623 = CARTESIAN_POINT ( 'NONE',  ( 4.699999999999995737, 7.505553499465141165, -1.387778780781445676E-14 ) ) ;
#7624 = DIRECTION ( 'NONE',  ( 0.000000000000000000, 1.000000000000000000, -0.000000000000000000 ) ) ;
#7625 = EDGE_LOOP ( 'NONE', ( #3994, #5071, #12126, #1988 ) ) ;
#7626 = DIRECTION ( 'NONE',  ( -5.204170427930409450E-16, 0.000000000000000000, 1.000000000000000000 ) ) ;
#7627 = DIRECTION ( 'NONE',  ( 1.000000000000000000, 0.000000000000000000, 0.000000000000000000 ) ) ;
#7628 = CARTESIAN_POINT ( 'NONE',  ( -68.99615306438083451, 96.25779118813026969, -167.1454815528550739 ) ) ;
#7629 = ORIENTED_EDGE ( 'NONE', *, *, #6459, .F. ) ;
#7630 = CARTESIAN_POINT ( 'NONE',  ( 0.000000000000000000, -91.08423613455721579, 0.000000000000000000 ) ) ;
#7631 = EDGE_LOOP ( 'NONE', ( #3962, #14623, #15735, #5842 ) ) ;
#7632 = LINE ( 'NONE', #14820, #7517 ) ;
#7633 = CARTESIAN_POINT ( 'NONE',  ( -66.76796488546020214, 108.3135598836077094, 24.99999999999999645 ) ) ;
#7634 = ORIENTED_EDGE ( 'NONE', *, *, #17708, .F. ) ;
#7635 = CIRCLE ( 'NONE', #7931, 4.599999999999999645 ) ;
#7636 = AXIS2_PLACEMENT_3D ( 'NONE', #1755, #7731, #17643 ) ;
#7637 = DIRECTION ( 'NONE',  ( 1.000000000000000000, 2.062304371594500494E-16, -0.000000000000000000 ) ) ;
#7638 = FACE_OUTER_BOUND ( 'NONE', #4229, .T. ) ;
#7639 = EDGE_LOOP ( 'NONE', ( #9375, #10956, #2585, #6009 ) ) ;
#7640 = VERTEX_POINT ( 'NONE', #1912 ) ;
#7641 = ORIENTED_EDGE ( 'NONE', *, *, #12007, .F. ) ;
#7642 = CARTESIAN_POINT ( 'NONE',  ( -71.24615306438117557, 5.970537365229261262, -15.00000000000001421 ) ) ;
#7643 = EDGE_CURVE ( 'NONE', #4979, #9931, #10504, .T. ) ;
#7644 = LINE ( 'NONE', #10641, #17192 ) ;
#7645 = DIRECTION ( 'NONE',  ( -1.000000000000000000, 0.000000000000000000, 0.000000000000000000 ) ) ;
#7646 = CARTESIAN_POINT ( 'NONE',  ( -67.59262256747315689, 50.58224449241410525, 35.00000000000000000 ) ) ;
#7647 = VERTEX_POINT ( 'NONE', #13331 ) ;
#7648 = DIRECTION ( 'NONE',  ( 0.9396926207859171987, 0.3420201433256444545, -1.086737899652999999E-16 ) ) ;
#7649 = CARTESIAN_POINT ( 'NONE',  ( -71.24615306438091977, 71.94398301522919326, -167.1454815528550739 ) ) ;
#7650 = CARTESIAN_POINT ( 'NONE',  ( -107.5926225674731711, 57.88796029049330372, -30.38417033480641294 ) ) ;
#7651 = CARTESIAN_POINT ( 'NONE',  ( 103.5381772159376084, -151.5628872026272802, 36.00000000000000711 ) ) ;
#7652 = CARTESIAN_POINT ( 'NONE',  ( 95.45835937779683888, -32.62665103886256190, 7.000000000000010658 ) ) ;
#7653 = ORIENTED_EDGE ( 'NONE', *, *, #15515, .F. ) ;
#7654 = CARTESIAN_POINT ( 'NONE',  ( 94.09522336508815954, 84.22855780814606419, 55.12736457073573604 ) ) ;
#7655 = EDGE_CURVE ( 'NONE', #11856, #18083, #6942, .T. ) ;
#7656 = ORIENTED_EDGE ( 'NONE', *, *, #15545, .F. ) ;
#7657 = ADVANCED_FACE ( 'NONE', ( #6192 ), #6032, .T. ) ;
#7658 = CARTESIAN_POINT ( 'NONE',  ( -66.46593056348568496, 59.53070700554641803, 24.99999999999999289 ) ) ;
#7659 = DIRECTION ( 'NONE',  ( 0.000000000000000000, -1.000000000000000000, 1.181335735494911869E-16 ) ) ;
#7660 = VERTEX_POINT ( 'NONE', #4794 ) ;
#7661 = ORIENTED_EDGE ( 'NONE', *, *, #14516, .T. ) ;
#7662 = ADVANCED_FACE ( 'NONE', ( #10699 ), #10517, .T. ) ;
#7663 = VERTEX_POINT ( 'NONE', #3396 ) ;
#7664 = EDGE_CURVE ( 'NONE', #8569, #12366, #10512, .T. ) ;
#7665 = EDGE_CURVE ( 'NONE', #12461, #10347, #13610, .T. ) ;
#7666 = DIRECTION ( 'NONE',  ( 0.000000000000000000, 0.000000000000000000, 1.000000000000000000 ) ) ;
#7667 = CARTESIAN_POINT ( 'NONE',  ( 0.000000000000000000, -5.629165124598996428, -3.250000000000020428 ) ) ;
#7668 = CARTESIAN_POINT ( 'NONE',  ( -74.36104963774657506, 107.9768795091070359, 23.30522882661994899 ) ) ;
#7669 = CARTESIAN_POINT ( 'NONE',  ( -64.89435165812551531, 90.86016871721213306, -15.00000000000001243 ) ) ;
#7670 = CARTESIAN_POINT ( 'NONE',  ( -71.24615306438087714, 69.69126110456377887, 15.00000000000006928 ) ) ;
#7671 = DIRECTION ( 'NONE',  ( 0.000000000000000000, 0.000000000000000000, 1.000000000000000000 ) ) ;
#7672 = ORIENTED_EDGE ( 'NONE', *, *, #10618, .F. ) ;
#7673 = ADVANCED_FACE ( 'NONE', ( #10793 ), #9638, .F. ) ;
#7674 = CARTESIAN_POINT ( 'NONE',  ( -68.99615306438080609, 108.2093059316626693, -167.1454815528550739 ) ) ;
#7675 = CARTESIAN_POINT ( 'NONE',  ( -75.91242157673514157, 61.69241362573040988, -27.61362678897647172 ) ) ;
#7676 = CARTESIAN_POINT ( 'NONE',  ( -68.99615306438072082, 127.6737176881302958, -167.1454815528550739 ) ) ;
#7677 = ORIENTED_EDGE ( 'NONE', *, *, #9852, .T. ) ;
#7678 = CARTESIAN_POINT ( 'NONE',  ( 97.91997734382704266, 84.22855780814606419, 62.50000000000001421 ) ) ;
#7679 = DIRECTION ( 'NONE',  ( 0.9396926207859171987, 0.3420201433256445100, 4.890320548438495251E-16 ) ) ;
#7680 = EDGE_CURVE ( 'NONE', #16077, #3860, #16491, .T. ) ;
#7681 = ORIENTED_EDGE ( 'NONE', *, *, #12311, .T. ) ;
#7682 = ADVANCED_FACE ( 'NONE', ( #6476 ), #12198, .T. ) ;
#7683 = VERTEX_POINT ( 'NONE', #9398 ) ;
#7684 = EDGE_CURVE ( 'NONE', #9812, #8044, #2274, .T. ) ;
#7685 = DIRECTION ( 'NONE',  ( -1.000000000000000000, -1.624875145807134646E-14, 1.692578276882432005E-16 ) ) ;
#7686 = CARTESIAN_POINT ( 'NONE',  ( -71.24615306438089135, 84.51035361522924916, -167.1454815528550739 ) ) ;
#7687 = CARTESIAN_POINT ( 'NONE',  ( -68.99615306438094819, 54.80223088166269463, -167.1454815528550739 ) ) ;
#7688 = ORIENTED_EDGE ( 'NONE', *, *, #6258, .T. ) ;
#7689 = FACE_OUTER_BOUND ( 'NONE', #16927, .T. ) ;
#7690 = ORIENTED_EDGE ( 'NONE', *, *, #17836, .F. ) ;
#7691 = ADVANCED_BREP_SHAPE_REPRESENTATION ( '', ( #6489, #16217 ), #17131 ) ;
#7692 = CARTESIAN_POINT ( 'NONE',  ( 0.2573354458088474295, -4.368923434677343565, -5.432802636760800219 ) ) ;
#7693 = FACE_OUTER_BOUND ( 'NONE', #214, .T. ) ;
#7694 = PLANE ( 'NONE',  #6057 ) ;
#7695 = CARTESIAN_POINT ( 'NONE',  ( -64.09025127992791226, 117.8748711238780373, 35.00000000000000000 ) ) ;
#7696 = VERTEX_POINT ( 'NONE', #5353 ) ;
#7697 = CARTESIAN_POINT ( 'NONE',  ( -123.4618227840623632, -151.5628872026273086, 18.23991632971911869 ) ) ;
#7698 = ORIENTED_EDGE ( 'NONE', *, *, #15703, .F. ) ;
#7699 = DIRECTION ( 'NONE',  ( 0.000000000000000000, 0.000000000000000000, 1.000000000000000000 ) ) ;
#7700 = ORIENTED_EDGE ( 'NONE', *, *, #7891, .T. ) ;
#7701 = ORIENTED_EDGE ( 'NONE', *, *, #4788, .F. ) ;
#7702 = ORIENTED_EDGE ( 'NONE', *, *, #2064, .T. ) ;
#7703 = DIRECTION ( 'NONE',  ( 1.000000000000000000, 0.000000000000000000, -0.000000000000000000 ) ) ;
#7704 = DIRECTION ( 'NONE',  ( 0.000000000000000000, -1.000000000000000000, 0.000000000000000000 ) ) ;
#7705 = VERTEX_POINT ( 'NONE', #1360 ) ;
#7706 = DIRECTION ( 'NONE',  ( 0.000000000000000000, 0.000000000000000000, 1.000000000000000000 ) ) ;
#7707 = DIRECTION ( 'NONE',  ( 0.000000000000000000, 1.000000000000000000, 0.000000000000000000 ) ) ;
#7708 = ORIENTED_EDGE ( 'NONE', *, *, #14542, .T. ) ;
#7709 = DIRECTION ( 'NONE',  ( -1.000000000000000000, -0.000000000000000000, -0.000000000000000000 ) ) ;
#7710 = ORIENTED_EDGE ( 'NONE', *, *, #5047, .T. ) ;
#7711 = FACE_OUTER_BOUND ( 'NONE', #1431, .T. ) ;
#7712 = CARTESIAN_POINT ( 'NONE',  ( -68.99615306438117557, 5.151604338130305827, 15.00000000000006928 ) ) ;
#7713 = VERTEX_POINT ( 'NONE', #4155 ) ;
#7714 = CARTESIAN_POINT ( 'NONE',  ( -70.71978124295696944, -111.0842361345572158, 5.204170427930421283E-15 ) ) ;
#7715 = CIRCLE ( 'NONE', #7145, 4.600000000000006750 ) ;
#7716 = CARTESIAN_POINT ( 'NONE',  ( -76.37409655828219002, -96.08423613455721579, -45.05044770573186952 ) ) ;
#7717 = ORIENTED_EDGE ( 'NONE', *, *, #6412, .T. ) ;
#7718 = EDGE_LOOP ( 'NONE', ( #7915, #13390, #3594 ) ) ;
#7719 = PRODUCT_DEFINITION_SHAPE ( 'NONE', 'NONE',  #18525 ) ;
#7720 = ORIENTED_EDGE ( 'NONE', *, *, #11353, .T. ) ;
#7721 = DIRECTION ( 'NONE',  ( 0.9396926207859092051, 0.3420201433256663259, 0.000000000000000000 ) ) ;
#7722 = DIRECTION ( 'NONE',  ( -1.000000000000000000, -0.000000000000000000, -0.000000000000000000 ) ) ;
#7723 = VERTEX_POINT ( 'NONE', #18282 ) ;
#7724 = APPLICATION_PROTOCOL_DEFINITION ( 'draft international standard', 'automotive_design', 1998, #12931 ) ;
#7725 = DIRECTION ( 'NONE',  ( 1.000000000000000000, 0.000000000000000000, 0.000000000000000000 ) ) ;
#7726 = DIRECTION ( 'NONE',  ( 0.000000000000000000, 0.000000000000000000, 1.000000000000000000 ) ) ;
#7727 = VECTOR ( 'NONE', #16989, 1000.000000000000000 ) ;
#7728 = CYLINDRICAL_SURFACE ( 'NONE', #3115, 4.599999999999992539 ) ;
#7729 = ORIENTED_EDGE ( 'NONE', *, *, #11909, .F. ) ;
#7730 = DIRECTION ( 'NONE',  ( 0.000000000000000000, 0.000000000000000000, -1.000000000000000000 ) ) ;
#7731 = DIRECTION ( 'NONE',  ( -1.000000000000000000, -4.124608743189000987E-16, 0.000000000000000000 ) ) ;
#7732 = CYLINDRICAL_SURFACE ( 'NONE', #11542, 12.50000000000000355 ) ;
#7733 = DIRECTION ( 'NONE',  ( -0.000000000000000000, -0.000000000000000000, -1.000000000000000000 ) ) ;
#7734 = DIRECTION ( 'NONE',  ( -1.000000000000000000, 0.000000000000000000, 0.000000000000000000 ) ) ;
#7735 = ORIENTED_EDGE ( 'NONE', *, *, #7562, .F. ) ;
#7736 = DIRECTION ( 'NONE',  ( 1.000000000000000000, 0.000000000000000000, 0.000000000000000000 ) ) ;
#7737 = CARTESIAN_POINT ( 'NONE',  ( -57.08002265617300708, 84.22855780814606419, 15.00000000000006928 ) ) ;
#7738 = EDGE_LOOP ( 'NONE', ( #12865, #6763, #9341, #5920, #8463 ) ) ;
#7739 = EDGE_CURVE ( 'NONE', #12217, #13329, #12495, .T. ) ;
#7740 = CYLINDRICAL_SURFACE ( 'NONE', #4493, 7.500000000000000000 ) ;
#7741 = DIRECTION ( 'NONE',  ( 0.000000000000000000, 0.000000000000000000, 1.000000000000000000 ) ) ;
#7742 = ORIENTED_EDGE ( 'NONE', *, *, #10405, .F. ) ;
#7743 = AXIS2_PLACEMENT_3D ( 'NONE', #3306, #7626, #62 ) ;
#7744 = VERTEX_POINT ( 'NONE', #12688 ) ;
#7745 = VECTOR ( 'NONE', #15195, 1000.000000000000114 ) ;
#7746 = CARTESIAN_POINT ( 'NONE',  ( -68.99615306438067819, 146.5232735881302801, -167.1454815528550739 ) ) ;
#7747 = ORIENTED_EDGE ( 'NONE', *, *, #16977, .T. ) ;
#7748 = CARTESIAN_POINT ( 'NONE',  ( -76.37409655828265898, -111.0842361345572158, -8.001217251689905290E-13 ) ) ;
#7749 = DIRECTION ( 'NONE',  ( 0.000000000000000000, 0.000000000000000000, 1.000000000000000000 ) ) ;
#7750 = EDGE_CURVE ( 'NONE', #14710, #2889, #11438, .T. ) ;
#7751 = CARTESIAN_POINT ( 'NONE',  ( -68.99615306438099083, 45.99230878813025925, -15.00000000000001421 ) ) ;
#7752 = LINE ( 'NONE', #12069, #5683 ) ;
#7753 = FACE_OUTER_BOUND ( 'NONE', #15590, .T. ) ;
#7754 = DIRECTION ( 'NONE',  ( 0.000000000000000000, 1.000000000000000000, 0.000000000000000000 ) ) ;
#7755 = EDGE_LOOP ( 'NONE', ( #16397, #8802, #15686, #15603, #4156, #10580 ) ) ;
#7756 = AXIS2_PLACEMENT_3D ( 'NONE', #7676, #2057, #6249 ) ;
#7757 = CARTESIAN_POINT ( 'NONE',  ( -71.24615306438086293, 87.65194626522927024, -15.00000000000001421 ) ) ;
#7758 = CARTESIAN_POINT ( 'NONE',  ( -76.11074570696128205, 61.85979623000802974, -25.83329931759948295 ) ) ;
#7759 = AXIS2_PLACEMENT_3D ( 'NONE', #16951, #11344, #7220 ) ;
#7760 = APPLICATION_CONTEXT ( 'automotive_design' ) ;
#7761 = LINE ( 'NONE', #7589, #14343 ) ;
#7762 = VERTEX_POINT ( 'NONE', #13985 ) ;
#7763 = EDGE_CURVE ( 'NONE', #18214, #7705, #1288, .T. ) ;
#7764 = EDGE_CURVE ( 'NONE', #15245, #17316, #15907, .T. ) ;
#7765 = B_SPLINE_CURVE_WITH_KNOTS ( 'NONE', 3,
 ( #6252, #16084, #11048, #18060 ),
 .UNSPECIFIED., .F., .F.,
 ( 4, 4 ),
 ( 0.000000000000000000, 0.002699315152504171492 ),
 .UNSPECIFIED. ) ;
#7766 = FACE_OUTER_BOUND ( 'NONE', #6738, .T. ) ;
#7767 = CARTESIAN_POINT ( 'NONE',  ( -66.35137518009933899, 89.78028827820979529, 15.00000000000006928 ) ) ;
#7768 = ORIENTED_EDGE ( 'NONE', *, *, #2250, .F. ) ;
#7769 = EDGE_CURVE ( 'NONE', #4352, #11429, #18186, .T. ) ;
#7770 = VECTOR ( 'NONE', #5880, 1000.000000000000114 ) ;
#7771 = ORIENTED_EDGE ( 'NONE', *, *, #9729, .F. ) ;
#7773 = EDGE_CURVE ( 'NONE', #16605, #17396, #3776, .T. ) ;
#7772 = VECTOR ( 'NONE', #8608, 1000.000000000000000 ) ;
#7774 = AXIS2_PLACEMENT_3D ( 'NONE', #12445, #12234, #17843 ) ;
#7775 = PLANE ( 'NONE',  #4866 ) ;
#7776 = CARTESIAN_POINT ( 'NONE',  ( 93.45071565215914688, 84.22855780814606419, 50.20642594383511437 ) ) ;
#7777 = ADVANCED_FACE ( 'NONE', ( #7066 ), #18385, .T. ) ;
#7778 = DIRECTION ( 'NONE',  ( 0.000000000000000000, 0.000000000000000000, 1.000000000000000000 ) ) ;
#7779 = PLANE ( 'NONE',  #16198 ) ;
#7780 = EDGE_CURVE ( 'NONE', #12181, #11983, #6328, .T. ) ;
#7781 = ORIENTED_EDGE ( 'NONE', *, *, #9740, .F. ) ;
#7782 = PLANE ( 'NONE',  #7175 ) ;
#7783 = ADVANCED_FACE ( 'NONE', ( #977 ), #11366, .T. ) ;
#7784 = ORIENTED_EDGE ( 'NONE', *, *, #577, .T. ) ;
#7785 = CARTESIAN_POINT ( 'NONE',  ( 0.05533025579369500735, -4.993776679986010159, -4.350525068611887036 ) ) ;
#7786 = CARTESIAN_POINT ( 'NONE',  ( -70.71978124295696944, -141.5628872026273086, 18.23991632971911869 ) ) ;
#7787 = DIRECTION ( 'NONE',  ( 0.000000000000000000, -1.000000000000000000, 0.000000000000000000 ) ) ;
#7788 = CARTESIAN_POINT ( 'NONE',  ( -67.79562744116532258, 82.83016482797231106, 15.00000000000006928 ) ) ;
#7789 = EDGE_LOOP ( 'NONE', ( #49, #3640, #16748, #990 ) ) ;
#7790 = AXIS2_PLACEMENT_3D ( 'NONE', #15129, #17840, #8016 ) ;
#7791 = CARTESIAN_POINT ( 'NONE',  ( -68.99615306438106188, 23.38630438166269698, -167.1454815528550739 ) ) ;
#7792 = ORIENTED_EDGE ( 'NONE', *, *, #9454, .F. ) ;
#7793 = ADVANCED_FACE ( 'NONE', ( #18473 ), #2468, .T. ) ;
#7794 = EDGE_CURVE ( 'NONE', #11906, #2577, #15177, .T. ) ;
#7795 = AXIS2_PLACEMENT_3D ( 'NONE', #1559, #1653, #17442 ) ;
#7796 = LINE ( 'NONE', #16661, #16365 ) ;
#7797 = ORIENTED_EDGE ( 'NONE', *, *, #4361, .T. ) ;
#7798 = ORIENTED_EDGE ( 'NONE', *, *, #15088, .T. ) ;
#7799 = VECTOR ( 'NONE', #7072, 1000.000000000000114 ) ;
#7800 = LINE ( 'NONE', #7978, #5810 ) ;
#7801 = CARTESIAN_POINT ( 'NONE',  ( -115.7702289486888247, -96.08423613455721579, 5.654315315325360913 ) ) ;
#7802 = ORIENTED_EDGE ( 'NONE', *, *, #924, .T. ) ;
#7803 = AXIS2_PLACEMENT_3D ( 'NONE', #10229, #14612, #8844 ) ;
#7804 = AXIS2_PLACEMENT_3D ( 'NONE', #4530, #7527, #10074 ) ;
#7805 = CARTESIAN_POINT ( 'NONE',  ( -123.4618227840623632, -151.5628872026273086, 57.00000000000000000 ) ) ;
#7806 = EDGE_CURVE ( 'NONE', #1716, #17497, #5644, .T. ) ;
#7807 = DIRECTION ( 'NONE',  ( 0.000000000000000000, 3.469446951953617344E-15, 1.000000000000000000 ) ) ;
#7808 = EDGE_LOOP ( 'NONE', ( #633, #11879, #866, #17954 ) ) ;
#7809 = DIRECTION ( 'NONE',  ( -4.163336342344339393E-15, 0.000000000000000000, 1.000000000000000000 ) ) ;
#7810 = VERTEX_POINT ( 'NONE', #3961 ) ;
#7811 = DIRECTION ( 'NONE',  ( -0.9396926207859022107, 0.3420201433256853663, 0.000000000000000000 ) ) ;
#7812 = LINE ( 'NONE', #7989, #3951 ) ;
#7813 = LINE ( 'NONE', #10708, #15386 ) ;
#7814 = DIRECTION ( 'NONE',  ( 0.000000000000000000, 0.000000000000000000, 1.000000000000000000 ) ) ;
#7815 = AXIS2_PLACEMENT_3D ( 'NONE', #755, #10472, #7671 ) ;
#7816 = EDGE_LOOP ( 'NONE', ( #6555, #8062, #17672, #17105 ) ) ;
#7817 = ORIENTED_EDGE ( 'NONE', *, *, #469, .T. ) ;
#7818 = LINE ( 'NONE', #13533, #2197 ) ;
#7819 = DIRECTION ( 'NONE',  ( 0.000000000000000000, 0.000000000000000000, 1.000000000000000000 ) ) ;
#7820 = EDGE_CURVE ( 'NONE', #4896, #13281, #13789, .T. ) ;
#7821 = AXIS2_PLACEMENT_3D ( 'NONE', #7271, #17443, #7440 ) ;
#7822 = ORIENTED_EDGE ( 'NONE', *, *, #6068, .F. ) ;
#7823 = DIRECTION ( 'NONE',  ( 1.000000000000000000, 0.000000000000000000, 0.000000000000000000 ) ) ;
#7824 = CARTESIAN_POINT ( 'NONE',  ( -54.93063083320800644, 106.4346967249107792, 102.5000000000000000 ) ) ;
#7825 = DIRECTION ( 'NONE',  ( 0.000000000000000000, 1.000000000000000000, 0.000000000000000000 ) ) ;
#7826 = ORIENTED_EDGE ( 'NONE', *, *, #16457, .F. ) ;
#7827 = DIRECTION ( 'NONE',  ( -0.9396926207859097602, 0.3420201433256649937, 1.086737899652991371E-16 ) ) ;
#7828 = CIRCLE ( 'NONE', #14687, 4.599999999999999645 ) ;
#7829 = VECTOR ( 'NONE', #17645, 1000.000000000000000 ) ;
#7830 = DIRECTION ( 'NONE',  ( 0.000000000000000000, 0.000000000000000000, 1.000000000000000000 ) ) ;
#7831 = CARTESIAN_POINT ( 'NONE',  ( -68.99615306438086293, 92.50134268166266338, -15.00000000000001421 ) ) ;
#7832 = DIRECTION ( 'NONE',  ( -1.000000000000000000, -2.062304371594500740E-16, -0.000000000000000000 ) ) ;
#7833 = ORIENTED_EDGE ( 'NONE', *, *, #7126, .T. ) ;
#7834 = CARTESIAN_POINT ( 'NONE',  ( -97.59262256747321373, 110.5691553257988460, -26.35917033480641436 ) ) ;
#7835 = PLANE ( 'NONE',  #11081 ) ;
#7836 = ORIENTED_EDGE ( 'NONE', *, *, #15548, .F. ) ;
#7837 = VECTOR ( 'NONE', #670, 1000.000000000000000 ) ;
#7838 = CARTESIAN_POINT ( 'NONE',  ( -68.99615306438080609, 105.6825691381303045, -167.1454815528550739 ) ) ;
#7839 =( NAMED_UNIT ( * ) SI_UNIT ( $, .STERADIAN. ) SOLID_ANGLE_UNIT ( ) );
#7840 = ORIENTED_EDGE ( 'NONE', *, *, #18366, .T. ) ;
#7841 = ADVANCED_FACE ( 'NONE', ( #10983 ), #16669, .T. ) ;
#7842 = ORIENTED_EDGE ( 'NONE', *, *, #17726, .T. ) ;
#7843 = CIRCLE ( 'NONE', #6959, 12.50000000000000355 ) ;
#7844 = VECTOR ( 'NONE', #13596, 1000.000000000000227 ) ;
#7845 = LINE ( 'NONE', #9526, #12960 ) ;
#7846 = ORIENTED_EDGE ( 'NONE', *, *, #18140, .F. ) ;
#7847 = DIRECTION ( 'NONE',  ( 0.000000000000000000, 0.000000000000000000, 1.000000000000000000 ) ) ;
#7848 = DIRECTION ( 'NONE',  ( 0.3420201433256444545, -0.9396926207859171987, 0.000000000000000000 ) ) ;
#7849 = CARTESIAN_POINT ( 'NONE',  ( -68.99615306438087714, 86.83301323813024908, -15.00000000000001421 ) ) ;
#7850 = CIRCLE ( 'NONE', #9048, 11.04359719766050141 ) ;
#7851 = DIRECTION ( 'NONE',  ( 0.000000000000000000, 0.000000000000000000, 1.000000000000000000 ) ) ;
#7852 = DIRECTION ( 'NONE',  ( 0.9396926207859171987, 0.3420201433256444545, -1.086737899652999999E-16 ) ) ;
#7853 = DIRECTION ( 'NONE',  ( 0.000000000000000000, 0.000000000000000000, 1.000000000000000000 ) ) ;
#7854 = ORIENTED_EDGE ( 'NONE', *, *, #16225, .T. ) ;
#7855 = CARTESIAN_POINT ( 'NONE',  ( -74.24049782422095234, 60.39151088118022415, -23.22272012184626178 ) ) ;
#7856 = VECTOR ( 'NONE', #5443, 1000.000000000000000 ) ;
#7857 = AXIS2_PLACEMENT_3D ( 'NONE', #12909, #3327, #13005 ) ;
#7858 = DIRECTION ( 'NONE',  ( 0.000000000000000000, 0.000000000000000000, -1.000000000000000000 ) ) ;
#7859 = ORIENTED_EDGE ( 'NONE', *, *, #8822, .F. ) ;
#7860 = CARTESIAN_POINT ( 'NONE',  ( -92.59262256747319952, 50.58224449241410525, 35.00000000000000000 ) ) ;
#7861 = DIRECTION ( 'NONE',  ( 0.000000000000000000, 1.000000000000000000, 0.000000000000000000 ) ) ;
#7862 = ORIENTED_EDGE ( 'NONE', *, *, #11873, .F. ) ;
#7863 = EDGE_CURVE ( 'NONE', #4718, #16572, #12653, .T. ) ;
#7864 = ORIENTED_EDGE ( 'NONE', *, *, #9489, .T. ) ;
#7865 = AXIS2_PLACEMENT_3D ( 'NONE', #10269, #15972, #2903 ) ;
#7866 = AXIS2_PLACEMENT_3D ( 'NONE', #11568, #10342, #3222 ) ;
#7867 = AXIS2_PLACEMENT_3D ( 'NONE', #2383, #15198, #1102 ) ;
#7868 = FACE_OUTER_BOUND ( 'NONE', #14090, .T. ) ;
#7869 = LINE ( 'NONE', #3475, #17988 ) ;
#7870 = FACE_OUTER_BOUND ( 'NONE', #9159, .T. ) ;
#7871 = CARTESIAN_POINT ( 'NONE',  ( -68.99615306438120399, -1.746436818337276931, 15.00000000000006928 ) ) ;
#7872 = VERTEX_POINT ( 'NONE', #6862 ) ;
#7873 = EDGE_CURVE ( 'NONE', #773, #15101, #16871, .T. ) ;
#7874 = DIRECTION ( 'NONE',  ( 0.000000000000000000, 1.000000000000000000, 0.000000000000000000 ) ) ;
#7875 = CARTESIAN_POINT ( 'NONE',  ( 0.000000000000000000, 5.629165124598635828, -3.250000000000016875 ) ) ;
#7876 =( REPRESENTATION_RELATIONSHIP ('NONE','NONE', #359, #17553 ) REPRESENTATION_RELATIONSHIP_WITH_TRANSFORMATION ( #10898 )SHAPE_REPRESENTATION_RELATIONSHIP( ) );
#7877 = ORIENTED_EDGE ( 'NONE', *, *, #4350, .F. ) ;
#7878 = FACE_OUTER_BOUND ( 'NONE', #14463, .T. ) ;
#7879 = FACE_OUTER_BOUND ( 'NONE', #13709, .T. ) ;
#7880 = DIRECTION ( 'NONE',  ( -1.000000000000000000, -2.062304371594500494E-16, -0.000000000000000000 ) ) ;
#7881 = CARTESIAN_POINT ( 'NONE',  ( -111.0396820472914214, -91.18731257919067446, 9.610190611755312418 ) ) ;
#7882 = ORIENTED_EDGE ( 'NONE', *, *, #16573, .T. ) ;
#7883 = DIRECTION ( 'NONE',  ( -1.000000000000000000, 0.000000000000000000, 0.000000000000000000 ) ) ;
#7884 = ORIENTED_EDGE ( 'NONE', *, *, #9260, .T. ) ;
#7885 = EDGE_CURVE ( 'NONE', #16082, #8820, #298, .T. ) ;
#7886 = VECTOR ( 'NONE', #14835, 1000.000000000000000 ) ;
#7887 = CARTESIAN_POINT ( 'NONE',  ( -68.99615306438097662, 57.94382353166266597, 15.00000000000006928 ) ) ;
#7889 = ORIENTED_EDGE ( 'NONE', *, *, #548, .T. ) ;
#7888 = VECTOR ( 'NONE', #11461, 1000.000000000000000 ) ;
#7890 = EDGE_CURVE ( 'NONE', #11836, #5685, #6086, .T. ) ;
#7891 = EDGE_CURVE ( 'NONE', #12615, #11278, #17057, .T. ) ;
#7892 = EDGE_LOOP ( 'NONE', ( #13127, #12312, #18356, #11192 ) ) ;
#7893 = LINE ( 'NONE', #3684, #2215 ) ;
#7894 = CARTESIAN_POINT ( 'NONE',  ( -68.99615306438083451, 101.9261206316626698, -167.1454815528550739 ) ) ;
#7895 = AXIS2_PLACEMENT_3D ( 'NONE', #7834, #11951, #10652 ) ;
#7896 = ADVANCED_FACE ( 'NONE', ( #1442 ), #16795, .T. ) ;
#7897 = EDGE_LOOP ( 'NONE', ( #5192, #11869, #9662, #13652 ) ) ;
#7898 = EDGE_CURVE ( 'NONE', #2089, #18486, #7147, .T. ) ;
#7899 = AXIS2_PLACEMENT_3D ( 'NONE', #4987, #6579, #10620 ) ;
#7900 = EDGE_CURVE ( 'NONE', #3688, #9785, #9937, .T. ) ;
#7901 = DIRECTION ( 'NONE',  ( 0.000000000000000000, 0.000000000000000000, 1.000000000000000000 ) ) ;
#7902 = CARTESIAN_POINT ( 'NONE',  ( -71.24615306438084872, 79.11603905456375685, 15.00000000000006928 ) ) ;
#7903 = ORIENTED_EDGE ( 'NONE', *, *, #16690, .T. ) ;
#7904 = EDGE_CURVE ( 'NONE', #7063, #15333, #7502, .T. ) ;
#7905 = CARTESIAN_POINT ( 'NONE',  ( 4.699999999999995737, -2.914335439641035919E-13, -6.500000000000019540 ) ) ;
#7906 = VERTEX_POINT ( 'NONE', #8643 ) ;
#7907 = DIRECTION ( 'NONE',  ( -5.204170427930409450E-16, 0.000000000000000000, 1.000000000000000000 ) ) ;
#7908 = DIRECTION ( 'NONE',  ( 0.000000000000000000, 1.000000000000000000, 0.000000000000000000 ) ) ;
#7909 = EDGE_CURVE ( 'NONE', #10207, #10372, #13219, .T. ) ;
#7910 = AXIS2_PLACEMENT_3D ( 'NONE', #3653, #4766, #567 ) ;
#7911 = FACE_OUTER_BOUND ( 'NONE', #8506, .T. ) ;
#7912 = AXIS2_PLACEMENT_3D ( 'NONE', #431, #12901, #12996 ) ;
#7913 = CARTESIAN_POINT ( 'NONE',  ( -80.06812138002644019, -91.24992890033503556, -40.65007677557141363 ) ) ;
#7914 = CIRCLE ( 'NONE', #18390, 21.04359719766050318 ) ;
#7915 = ORIENTED_EDGE ( 'NONE', *, *, #9750, .T. ) ;
#7916 = EDGE_CURVE ( 'NONE', #7225, #14192, #10223, .T. ) ;
#7917 = VECTOR ( 'NONE', #5410, 1000.000000000000000 ) ;
#7918 = EDGE_CURVE ( 'NONE', #11153, #15074, #398, .T. ) ;
#7919 = ORIENTED_EDGE ( 'NONE', *, *, #18069, .F. ) ;
#7920 = CARTESIAN_POINT ( 'NONE',  ( -83.12361985383350316, 84.22855780814606419, 37.50000000000000000 ) ) ;
#7921 = DIRECTION ( 'NONE',  ( -0.9396926207859084279, 0.3420201433256687684, 1.086737899652989769E-16 ) ) ;
#7922 = ORIENTED_EDGE ( 'NONE', *, *, #10903, .F. ) ;
#7923 = CARTESIAN_POINT ( 'NONE',  ( -64.75543355702687620, 94.09456345901884333, 15.00000000000006928 ) ) ;
#7924 = CARTESIAN_POINT ( 'NONE',  ( -107.5926225674731711, 57.88796029049330372, -22.35917033480642502 ) ) ;
#7925 = CARTESIAN_POINT ( 'NONE',  ( 2.371465054068948142, 0.7538881668847053907, 50.31856894691938464 ) ) ;
#7926 = EDGE_CURVE ( 'NONE', #6312, #17387, #4605, .T. ) ;
#7927 = DIRECTION ( 'NONE',  ( 0.000000000000000000, -0.000000000000000000, -1.000000000000000000 ) ) ;
#7928 = ORIENTED_EDGE ( 'NONE', *, *, #47, .T. ) ;
#7929 = CIRCLE ( 'NONE', #18402, 9.999999999999994671 ) ;
#7930 = DIRECTION ( 'NONE',  ( -2.062304371594500494E-16, 1.000000000000000000, 0.000000000000000000 ) ) ;
#7931 = AXIS2_PLACEMENT_3D ( 'NONE', #6321, #17748, #7462 ) ;
#7932 = FACE_OUTER_BOUND ( 'NONE', #8870, .T. ) ;
#7933 =( NAMED_UNIT ( * ) SI_UNIT ( $, .STERADIAN. ) SOLID_ANGLE_UNIT ( ) );
#7934 = VECTOR ( 'NONE', #9059, 1000.000000000000000 ) ;
#7935 = CARTESIAN_POINT ( 'NONE',  ( -71.24615306438097662, 59.37761241522920841, -15.00000000000001421 ) ) ;
#7936 = VERTEX_POINT ( 'NONE', #8561 ) ;
#7937 = LINE ( 'NONE', #10729, #8804 ) ;
#7938 = DIRECTION ( 'NONE',  ( 1.000000000000000000, 0.000000000000000000, 0.000000000000000000 ) ) ;
#7939 = EDGE_LOOP ( 'NONE', ( #5993, #7889, #10359, #6886 ) ) ;
#7940 = CARTESIAN_POINT ( 'NONE',  ( -68.99615306438097662, 58.55867938813025830, -15.00000000000001421 ) ) ;
#7941 = CARTESIAN_POINT ( 'NONE',  ( -37.32701571189549838, 76.97167339262615826, 64.45706195283406714 ) ) ;
#7942 = EDGE_LOOP ( 'NONE', ( #10784, #17136, #1158, #10473 ) ) ;
#7943 = EDGE_LOOP ( 'NONE', ( #6625, #8273, #4843, #15400 ) ) ;
#7944 = LINE ( 'NONE', #7746, #15928 ) ;
#7945 = ORIENTED_EDGE ( 'NONE', *, *, #11111, .F. ) ;
#7946 = DIRECTION ( 'NONE',  ( -1.000000000000000000, -0.000000000000000000, -0.000000000000000000 ) ) ;
#7947 = CARTESIAN_POINT ( 'NONE',  ( -68.99615306438060713, 143.3816809381303301, 15.00000000000006928 ) ) ;
#7948 = CARTESIAN_POINT ( 'NONE',  ( -67.59262256747315689, 129.5689604715732912, 15.00000000000005862 ) ) ;
#7949 = CARTESIAN_POINT ( 'NONE',  ( -57.08002265617300708, 84.22855780814606419, -35.00000000000000000 ) ) ;
#7950 = DIRECTION ( 'NONE',  ( -5.204170427930409450E-16, 0.000000000000000000, 1.000000000000000000 ) ) ;
#7951 = CARTESIAN_POINT ( 'NONE',  ( -66.35137518009933899, 89.78028827820979529, -167.1454815528550739 ) ) ;
#7952 = ORIENTED_EDGE ( 'NONE', *, *, #17757, .F. ) ;
#7953 = EDGE_CURVE ( 'NONE', #2278, #11754, #3121, .T. ) ;
#7954 = CARTESIAN_POINT ( 'NONE',  ( -107.5926225674732137, 117.8748711238780373, -25.00000000000000000 ) ) ;
#7955 = CARTESIAN_POINT ( 'NONE',  ( -68.99615306438072082, 140.2400882881302948, -15.00000000000001421 ) ) ;
#7956 = ORIENTED_EDGE ( 'NONE', *, *, #5023, .F. ) ;
#7957 = CARTESIAN_POINT ( 'NONE',  ( -28.16748190072492974, -91.96845925178433845, -7.798233810088249562 ) ) ;
#7958 = CARTESIAN_POINT ( 'NONE',  ( -98.90286936182235422, -96.08423613455721579, -2.027180301682503564E-13 ) ) ;
#7959 = ORIENTED_EDGE ( 'NONE', *, *, #17032, .F. ) ;
#7960 = ORIENTED_EDGE ( 'NONE', *, *, #17144, .F. ) ;
#7961 = LINE ( 'NONE', #6359, #15354 ) ;
#7962 = CARTESIAN_POINT ( 'NONE',  ( -68.99615306438089135, 67.36860148166267948, -15.00000000000001421 ) ) ;
#7963 = DIRECTION ( 'NONE',  ( 0.000000000000000000, 0.000000000000000000, -1.000000000000000000 ) ) ;
#7964 = DIRECTION ( 'NONE',  ( -1.000000000000000000, -0.000000000000000000, -0.000000000000000000 ) ) ;
#7965 = CARTESIAN_POINT ( 'NONE',  ( 95.45835937779683888, -32.62665103886256190, -7.000000000000010658 ) ) ;
#7966 = EDGE_LOOP ( 'NONE', ( #3380, #5119, #3833, #9811 ) ) ;
#7967 = CARTESIAN_POINT ( 'NONE',  ( -71.24615306438070661, 147.3422066152292871, -15.00000000000001421 ) ) ;
#7968 = CARTESIAN_POINT ( 'NONE',  ( -53.44605150580733266, 72.26844686893191749, -167.1454815528550739 ) ) ;
#7969 = DIRECTION ( 'NONE',  ( 1.156482317317869999E-16, 0.000000000000000000, 1.000000000000000000 ) ) ;
#7970 = CARTESIAN_POINT ( 'NONE',  ( -113.2720846013049822, -91.96846159163192169, 7.798230460770113837 ) ) ;
#7971 = ORIENTED_EDGE ( 'NONE', *, *, #16116, .F. ) ;
#7972 = CARTESIAN_POINT ( 'NONE',  ( -71.24615306438103346, 41.41692725456378099, -167.1454815528550739 ) ) ;
#7973 = ORIENTED_EDGE ( 'NONE', *, *, #2778, .T. ) ;
#7974 = DIRECTION ( 'NONE',  ( -0.9396926207859167546, 0.3420201433256455648, -4.890320548438493279E-16 ) ) ;
#7975 = VERTEX_POINT ( 'NONE', #5826 ) ;
#7976 = EDGE_CURVE ( 'NONE', #18067, #1261, #14265, .T. ) ;
#7977 = ORIENTED_EDGE ( 'NONE', *, *, #11005, .T. ) ;
#7978 = CARTESIAN_POINT ( 'NONE',  ( -107.5926225674731853, 50.58224449241411236, -25.00000000000000000 ) ) ;
#7979 = DIRECTION ( 'NONE',  ( 0.000000000000000000, 0.000000000000000000, 1.000000000000000000 ) ) ;
#7980 = ORIENTED_EDGE ( 'NONE', *, *, #18089, .F. ) ;
#7981 = CARTESIAN_POINT ( 'NONE',  ( -68.99615306438110451, 11.43478963813029381, -15.00000000000001421 ) ) ;
#7982 = EDGE_CURVE ( 'NONE', #5337, #10909, #5750, .T. ) ;
#7983 = PLANE ( 'NONE',  #1054 ) ;
#7984 = ORIENTED_EDGE ( 'NONE', *, *, #469, .F. ) ;
#7985 = SURFACE_STYLE_FILL_AREA ( #9683 ) ;
#7986 = CARTESIAN_POINT ( 'NONE',  ( -57.08002265617300708, 84.22855780814606419, -35.00000000000000000 ) ) ;
#7987 = ORIENTED_EDGE ( 'NONE', *, *, #13606, .T. ) ;
#7988 = CARTESIAN_POINT ( 'NONE',  ( -74.87319944600693589, 107.5944659956890632, -23.67920958164899048 ) ) ;
#7989 = CARTESIAN_POINT ( 'NONE',  ( -71.24615306438114715, 15.39531531522927921, 15.00000000000006928 ) ) ;
#7990 = VERTEX_POINT ( 'NONE', #1704 ) ;
#7991 = FACE_OUTER_BOUND ( 'NONE', #2353, .T. ) ;
#7992 = EDGE_CURVE ( 'NONE', #16431, #3688, #7409, .T. ) ;
#7993 = ADVANCED_FACE ( 'NONE', ( #8740 ), #2936, .T. ) ;
#7994 = CARTESIAN_POINT ( 'NONE',  ( -80.72210053294847398, -91.12516209206945916, -39.81919198398661308 ) ) ;
#7995 = ORIENTED_EDGE ( 'NONE', *, *, #3608, .T. ) ;
#7996 = ORIENTED_EDGE ( 'NONE', *, *, #489, .T. ) ;
#7997 = CIRCLE ( 'NONE', #841, 4.599999999999999645 ) ;
#7998 = DIRECTION ( 'NONE',  ( 0.9396926207859185309, 0.3420201433256406798, 4.890320548438501168E-16 ) ) ;
#7999 = DIRECTION ( 'NONE',  ( 0.000000000000000000, 0.000000000000000000, 1.000000000000000000 ) ) ;
#8000 = EDGE_CURVE ( 'NONE', #1867, #4994, #12963, .T. ) ;
#8001 = VERTEX_POINT ( 'NONE', #10132 ) ;
#8002 = CARTESIAN_POINT ( 'NONE',  ( -77.98774719866210603, 81.79799583099486426, 55.38794294486089598 ) ) ;
#8003 = DIRECTION ( 'NONE',  ( 0.000000000000000000, 0.000000000000000000, 1.000000000000000000 ) ) ;
#8004 = EDGE_CURVE ( 'NONE', #11612, #13941, #1624, .T. ) ;
#8005 = DIRECTION ( 'NONE',  ( -0.000000000000000000, -0.000000000000000000, -1.000000000000000000 ) ) ;
#8006 = ORIENTED_EDGE ( 'NONE', *, *, #10063, .F. ) ;
#8007 = DIRECTION ( 'NONE',  ( 0.000000000000000000, 0.000000000000000000, -1.000000000000000000 ) ) ;
#8008 = DIRECTION ( 'NONE',  ( 0.3420201433256686574, -0.9396926207859084279, 0.000000000000000000 ) ) ;
#8009 = EDGE_CURVE ( 'NONE', #299, #293, #1893, .T. ) ;
#8010 = CARTESIAN_POINT ( 'NONE',  ( -68.99615306438091977, 77.40823528813029952, -167.1454815528550739 ) ) ;
#8011 = EDGE_CURVE ( 'NONE', #15821, #15944, #15070, .T. ) ;
#8012 = AXIS2_PLACEMENT_3D ( 'NONE', #10125, #2061, #17779 ) ;
#8013 = CARTESIAN_POINT ( 'NONE',  ( -64.09025127992791226, 117.8748711238780373, 35.00000000000000000 ) ) ;
#8014 = ORIENTED_EDGE ( 'NONE', *, *, #8358, .T. ) ;
#8015 = LINE ( 'NONE', #3726, #16291 ) ;
#8016 = DIRECTION ( 'NONE',  ( -0.9396926207859097602, 0.3420201433256649937, 0.000000000000000000 ) ) ;
#8017 = ORIENTED_EDGE ( 'NONE', *, *, #1415, .F. ) ;
#8018 = ADVANCED_FACE ( 'NONE', ( #11820 ), #14697, .T. ) ;
#8019 = DIRECTION ( 'NONE',  ( 1.000000000000000000, 0.000000000000000000, 0.000000000000000000 ) ) ;
#8020 = CARTESIAN_POINT ( 'NONE',  ( -37.27426920733778104, 77.11479169650115750, 64.92672983002162823 ) ) ;
#8021 = ORIENTED_EDGE ( 'NONE', *, *, #2571, .F. ) ;
#8022 = ORIENTED_EDGE ( 'NONE', *, *, #14579, .T. ) ;
#8023 = CIRCLE ( 'NONE', #8635, 4.599999999999999645 ) ;
#8024 = CARTESIAN_POINT ( 'NONE',  ( -33.72855994630469212, 78.95224028009285178, 102.5000000000000000 ) ) ;
#8025 = EDGE_LOOP ( 'NONE', ( #7836, #13504, #14531, #17415 ) ) ;
#8026 = DIRECTION ( 'NONE',  ( -1.000000000000000000, -0.000000000000000000, -0.000000000000000000 ) ) ;
#8027 = CARTESIAN_POINT ( 'NONE',  ( -68.99615306438077766, 111.9657544381302330, -167.1454815528550739 ) ) ;
#8028 = CARTESIAN_POINT ( 'NONE',  ( 5.699999999999996625, -2.442490654175344586E-16, -4.400000000000027889 ) ) ;
#8029 = FACE_OUTER_BOUND ( 'NONE', #97, .T. ) ;
#8030 = FACE_OUTER_BOUND ( 'NONE', #12464, .T. ) ;
#8031 = DIRECTION ( 'NONE',  ( 1.000000000000000000, 2.062304371594500494E-16, 0.000000000000000000 ) ) ;
#8032 = DIRECTION ( 'NONE',  ( 0.000000000000000000, 1.000000000000000000, 0.000000000000000000 ) ) ;
#8033 = EDGE_LOOP ( 'NONE', ( #4471, #330, #3550, #2997, #15851 ) ) ;
#8034 = ADVANCED_FACE ( 'NONE', ( #9100 ), #4545, .T. ) ;
#8035 = DIRECTION ( 'NONE',  ( 0.000000000000000000, 0.000000000000000000, 1.000000000000000000 ) ) ;
#8036 = DIRECTION ( 'NONE',  ( 0.000000000000000000, 0.000000000000000000, -1.000000000000000000 ) ) ;
#8037 = VECTOR ( 'NONE', #17914, 1000.000000000000000 ) ;
#8038 = VERTEX_POINT ( 'NONE', #492 ) ;
#8039 = FACE_OUTER_BOUND ( 'NONE', #17196, .T. ) ;
#8040 = AXIS2_PLACEMENT_3D ( 'NONE', #7370, #13083, #10353 ) ;
#8041 = CARTESIAN_POINT ( 'NONE',  ( -57.08002265617300708, 84.22855780814606419, -15.00000000000001421 ) ) ;
#8042 = VERTEX_POINT ( 'NONE', #6263 ) ;
#8043 = ORIENTED_EDGE ( 'NONE', *, *, #10762, .F. ) ;
#8044 = VERTEX_POINT ( 'NONE', #11895 ) ;
#8045 = FACE_OUTER_BOUND ( 'NONE', #8690, .T. ) ;
#8046 = LINE ( 'NONE', #16561, #4844 ) ;
#8047 = AXIS2_PLACEMENT_3D ( 'NONE', #4263, #147, #5654 ) ;
#8048 = DIRECTION ( 'NONE',  ( -5.204170427930409450E-16, 0.000000000000000000, 1.000000000000000000 ) ) ;
#8049 = CARTESIAN_POINT ( 'NONE',  ( 103.5381772159376084, 0.000000000000000000, 57.00000000000000000 ) ) ;
#8050 = CARTESIAN_POINT ( 'NONE',  ( -71.24615306438067819, 144.2006139652292518, 15.00000000000006928 ) ) ;
#8051 = AXIS2_PLACEMENT_3D ( 'NONE', #15649, #2922, #18462 ) ;
#8052 = DIRECTION ( 'NONE',  ( 0.000000000000000000, 1.000000000000000000, 0.000000000000000000 ) ) ;
#8053 = ORIENTED_EDGE ( 'NONE', *, *, #8346, .T. ) ;
#8054 = DIRECTION ( 'NONE',  ( 1.000000000000000000, -0.000000000000000000, -0.000000000000000000 ) ) ;
#8055 = LINE ( 'NONE', #9557, #2138 ) ;
#8057 = ORIENTED_EDGE ( 'NONE', *, *, #14385, .F. ) ;
#8056 = CARTESIAN_POINT ( 'NONE',  ( -77.98770377200993664, 86.65978693925960386, 55.38805143041505374 ) ) ;
#8058 = CARTESIAN_POINT ( 'NONE',  ( 0.000000000000000000, -2.914335439641035919E-13, -6.500000000000019540 ) ) ;
#8059 = DIRECTION ( 'NONE',  ( 0.000000000000000000, 1.000000000000000000, 0.000000000000000000 ) ) ;
#8060 = ORIENTED_EDGE ( 'NONE', *, *, #5994, .F. ) ;
#8061 = FACE_OUTER_BOUND ( 'NONE', #14728, .T. ) ;
#8062 = ORIENTED_EDGE ( 'NONE', *, *, #12747, .T. ) ;
#8063 = CIRCLE ( 'NONE', #892, 20.99999999999999645 ) ;
#8064 = CIRCLE ( 'NONE', #11, 4.962965561209093046 ) ;
#8065 = VECTOR ( 'NONE', #5019, 1000.000000000000000 ) ;
#8066 = EDGE_CURVE ( 'NONE', #18486, #8399, #3284, .T. ) ;
#8067 = EDGE_LOOP ( 'NONE', ( #707, #12294, #5255, #6099, #15217, #12262 ) ) ;
#8068 = DIRECTION ( 'NONE',  ( -5.204170427930409450E-16, 0.000000000000000000, 1.000000000000000000 ) ) ;
#8069 = DIRECTION ( 'NONE',  ( 0.000000000000000000, 0.000000000000000000, -1.000000000000000000 ) ) ;
#8070 = VERTEX_POINT ( 'NONE', #16185 ) ;
#8071 = APPLICATION_PROTOCOL_DEFINITION ( 'draft international standard', 'automotive_design', 1998, #17428 ) ;
#8072 = PRESENTATION_LAYER_ASSIGNMENT (  '', '', ( #15852 ) ) ;
#8073 = DIRECTION ( 'NONE',  ( -1.000000000000000000, -0.000000000000000000, -0.000000000000000000 ) ) ;
#8074 = VECTOR ( 'NONE', #11523, 1000.000000000000000 ) ;
#8075 = LINE ( 'NONE', #12019, #15377 ) ;
#8076 = ORIENTED_EDGE ( 'NONE', *, *, #7684, .F. ) ;
#8077 = DIRECTION ( 'NONE',  ( 1.000000000000000000, 0.000000000000000000, 0.000000000000000000 ) ) ;
#8078 = LINE ( 'NONE', #16775, #5093 ) ;
#8079 = DIRECTION ( 'NONE',  ( 0.000000000000000000, 0.000000000000000000, 1.000000000000000000 ) ) ;
#8080 = AXIS2_PLACEMENT_3D ( 'NONE', #628, #17831, #8007 ) ;
#8081 = ORIENTED_EDGE ( 'NONE', *, *, #14440, .T. ) ;
#8082 = AXIS2_PLACEMENT_3D ( 'NONE', #12808, #14022, #9904 ) ;
#8083 = CARTESIAN_POINT ( 'NONE',  ( -75.55027201341330567, 107.0628432229694340, -24.42475462179574919 ) ) ;
#8084 = CARTESIAN_POINT ( 'NONE',  ( -71.24615306438097662, 59.37761241522920841, 15.00000000000006928 ) ) ;
#8085 = VERTEX_POINT ( 'NONE', #16372 ) ;
#8086 = DIRECTION ( 'NONE',  ( -0.000000000000000000, -0.000000000000000000, -1.000000000000000000 ) ) ;
#8087 = CARTESIAN_POINT ( 'NONE',  ( -68.99615306438111872, 20.85956758813031797, 15.00000000000006928 ) ) ;
#8088 = ORIENTED_EDGE ( 'NONE', *, *, #8488, .T. ) ;
#8089 = EDGE_CURVE ( 'NONE', #13449, #8653, #6969, .T. ) ;
#8090 = CIRCLE ( 'NONE', #10482, 10.24900000000000055 ) ;
#8091 = VECTOR ( 'NONE', #15099, 1000.000000000000000 ) ;
#8092 = CARTESIAN_POINT ( 'NONE',  ( -68.99615306438103346, 33.42593818813029571, -167.1454815528550739 ) ) ;
#8093 = LINE ( 'NONE', #16510, #15326 ) ;
#8094 = ORIENTED_EDGE ( 'NONE', *, *, #16008, .T. ) ;
#8095 = LINE ( 'NONE', #5297, #13766 ) ;
#8096 = CARTESIAN_POINT ( 'NONE',  ( -77.26565842541029383, 78.27883601870418318, 57.92718427577206342 ) ) ;
#8097 = CYLINDRICAL_SURFACE ( 'NONE', #18011, 85.91469608272775815 ) ;
#8098 = PLANE ( 'NONE',  #7296 ) ;
#8099 = VERTEX_POINT ( 'NONE', #14793 ) ;
#8100 = EDGE_CURVE ( 'NONE', #5068, #10635, #10772, .T. ) ;
#8101 = CARTESIAN_POINT ( 'NONE',  ( -68.99615306438099083, 36.56753083813024574, 15.00000000000006928 ) ) ;
#8102 = CARTESIAN_POINT ( 'NONE',  ( -60.62932119839002354, 94.43552448259767118, -167.1454815528550739 ) ) ;
#8103 = CARTESIAN_POINT ( 'NONE',  ( -48.21445538031289857, 89.37090336996882911, -15.00000000000001421 ) ) ;
#8104 = ADVANCED_FACE ( 'NONE', ( #17508 ), #17406, .T. ) ;
#8105 = DIRECTION ( 'NONE',  ( 0.3420201433256635504, 0.9396926207859103153, -0.000000000000000000 ) ) ;
#8106 = LINE ( 'NONE', #5014, #8730 ) ;
#8107 = ORIENTED_EDGE ( 'NONE', *, *, #9260, .F. ) ;
#8108 = EDGE_CURVE ( 'NONE', #13982, #4718, #5757, .T. ) ;
#8109 = AXIS2_PLACEMENT_3D ( 'NONE', #13017, #191, #10370 ) ;
#8110 = VECTOR ( 'NONE', #11898, 1000.000000000000000 ) ;
#8111 = CARTESIAN_POINT ( 'NONE',  ( -55.64822083176820655, 96.64628479562776420, 15.00000000000006928 ) ) ;
#8112 = LINE ( 'NONE', #16526, #16131 ) ;
#8113 = EDGE_LOOP ( 'NONE', ( #683, #16919, #435, #9515 ) ) ;
#8114 = DIRECTION ( 'NONE',  ( 0.000000000000000000, 0.000000000000000000, -1.000000000000000000 ) ) ;
#8115 = EDGE_CURVE ( 'NONE', #16289, #16963, #2175, .T. ) ;
#8116 = CARTESIAN_POINT ( 'NONE',  ( -36.05803663064089903, 83.24379415027478046, 69.93918222302725951 ) ) ;
#8117 = ORIENTED_EDGE ( 'NONE', *, *, #5854, .T. ) ;
#8118 = EDGE_CURVE ( 'NONE', #4518, #6934, #3377, .T. ) ;
#8119 = ORIENTED_EDGE ( 'NONE', *, *, #13726, .F. ) ;
#8120 = ADVANCED_FACE ( 'NONE', ( #3657 ), #7779, .T. ) ;
#8121 = AXIS2_PLACEMENT_3D ( 'NONE', #4632, #17347, #6022 ) ;
#8122 = DIRECTION ( 'NONE',  ( -2.062304371594500494E-16, 1.000000000000000000, -0.000000000000000000 ) ) ;
#8123 = ORIENTED_EDGE ( 'NONE', *, *, #10634, .T. ) ;
#8124 = VECTOR ( 'NONE', #17348, 1000.000000000000000 ) ;
#8125 = VECTOR ( 'NONE', #10848, 1000.000000000000000 ) ;
#8126 = DIRECTION ( 'NONE',  ( 0.000000000000000000, 1.000000000000000000, 0.000000000000000000 ) ) ;
#8127 = CARTESIAN_POINT ( 'NONE',  ( -47.76628296033400289, 88.50596986196467242, -167.1454815528550739 ) ) ;
#8128 = CARTESIAN_POINT ( 'NONE',  ( -64.09025127992791226, 117.8748711238780373, 35.00000000000000000 ) ) ;
#8129 = EDGE_CURVE ( 'NONE', #10654, #3050, #2474, .T. ) ;
#8130 = EDGE_CURVE ( 'NONE', #18088, #3227, #17685, .T. ) ;
#8131 = FACE_OUTER_BOUND ( 'NONE', #15757, .T. ) ;
#8132 = EDGE_CURVE ( 'NONE', #10671, #3670, #1986, .T. ) ;
#8133 = FACE_OUTER_BOUND ( 'NONE', #14586, .T. ) ;
#8134 = DIRECTION ( 'NONE',  ( 1.156482317317869999E-16, 0.000000000000000000, 1.000000000000000000 ) ) ;
#8135 = ORIENTED_EDGE ( 'NONE', *, *, #7863, .T. ) ;
#8136 = AXIS2_PLACEMENT_3D ( 'NONE', #7599, #12091, #10681 ) ;
#8137 = ADVANCED_FACE ( 'NONE', ( #4874 ), #10594, .T. ) ;
#8138 = CARTESIAN_POINT ( 'NONE',  ( 4.699999999999995737, -4.857225732735059864E-14, 6.500000000000037303 ) ) ;
#8139 = DIRECTION ( 'NONE',  ( 1.000000000000000000, 0.000000000000000000, 0.000000000000000000 ) ) ;
#8140 = ORIENTED_EDGE ( 'NONE', *, *, #6429, .F. ) ;
#8141 = CIRCLE ( 'NONE', #8754, 7.500000000000000000 ) ;
#8142 = CARTESIAN_POINT ( 'NONE',  ( -30.39988730823796104, -91.18731141006421126, -9.610196039195443518 ) ) ;
#8143 = VECTOR ( 'NONE', #14255, 1000.000000000000000 ) ;
#8144 = CARTESIAN_POINT ( 'NONE',  ( -57.08002265617300708, 84.22855780814606419, 15.00000000000006928 ) ) ;
#8145 = ORIENTED_EDGE ( 'NONE', *, *, #466, .T. ) ;
#8146 = ORIENTED_EDGE ( 'NONE', *, *, #14960, .T. ) ;
#8147 = ADVANCED_FACE ( 'NONE', ( #2072 ), #15258, .T. ) ;
#8148 = EDGE_CURVE ( 'NONE', #9163, #1951, #15456, .T. ) ;
#8149 = VERTEX_POINT ( 'NONE', #18164 ) ;
#8150 = VECTOR ( 'NONE', #1486, 1000.000000000000000 ) ;
#8151 = CARTESIAN_POINT ( 'NONE',  ( 124.5381772159375942, -151.5628872026272802, 36.00000000000001421 ) ) ;
#8152 = FACE_OUTER_BOUND ( 'NONE', #6494, .T. ) ;
#8153 = LINE ( 'NONE', #12276, #4012 ) ;
#8154 = LINE ( 'NONE', #16852, #11453 ) ;
#8155 = AXIS2_PLACEMENT_3D ( 'NONE', #1770, #7477, #9171 ) ;
#8156 = DIRECTION ( 'NONE',  ( 1.000000000000000000, 4.675871521838984962E-16, -0.000000000000000000 ) ) ;
#8157 = AXIS2_PLACEMENT_3D ( 'NONE', #15199, #7722, #7819 ) ;
#8158 = CIRCLE ( 'NONE', #9073, 11.04359719766049430 ) ;
#8159 = DIRECTION ( 'NONE',  ( 0.000000000000000000, 0.000000000000000000, 1.000000000000000000 ) ) ;
#8160 = EDGE_LOOP ( 'NONE', ( #6281, #6350, #2514, #16313, #8520 ) ) ;
#8161 = CARTESIAN_POINT ( 'NONE',  ( -71.24615306438100504, 49.95283446522918780, -167.1454815528550739 ) ) ;
#8162 = LINE ( 'NONE', #10876, #13194 ) ;
#8164 = VERTEX_POINT ( 'NONE', #87 ) ;
#8163 = CARTESIAN_POINT ( 'NONE',  ( -76.81489782590004722, 91.53406102980444814, 64.21492685509633702 ) ) ;
#8165 = DIRECTION ( 'NONE',  ( -1.000000000000000000, -0.000000000000000000, -0.000000000000000000 ) ) ;
#8166 = LINE ( 'NONE', #5446, #6567 ) ;
#8167 = EDGE_LOOP ( 'NONE', ( #15943, #8123, #3773, #4420 ) ) ;
#8168 = AXIS2_PLACEMENT_3D ( 'NONE', #3992, #16990, #7089 ) ;
#8169 = ORIENTED_EDGE ( 'NONE', *, *, #4143, .T. ) ;
#8170 = EDGE_CURVE ( 'NONE', #15520, #6455, #2556, .T. ) ;
#8171 =( GEOMETRIC_REPRESENTATION_CONTEXT ( 3 ) GLOBAL_UNCERTAINTY_ASSIGNED_CONTEXT ( ( #18256 ) ) GLOBAL_UNIT_ASSIGNED_CONTEXT ( ( #11672, #1668, #7550 ) ) REPRESENTATION_CONTEXT ( 'NONE', 'WORKASPACE' ) );
#8172 = CIRCLE ( 'NONE', #7584, 4.999999999999997335 ) ;
#8173 = ORIENTED_EDGE ( 'NONE', *, *, #14863, .T. ) ;
#8174 = CARTESIAN_POINT ( 'NONE',  ( -102.4618227840623774, -111.0842361345572158, -57.00000000000000000 ) ) ;
#8175 = PLANE ( 'NONE',  #6358 ) ;
#8176 = DIRECTION ( 'NONE',  ( 1.000000000000000000, 0.000000000000000000, 3.771137991253928573E-16 ) ) ;
#8177 = ORIENTED_EDGE ( 'NONE', *, *, #3089, .F. ) ;
#8178 = ITEM_DEFINED_TRANSFORMATION ( 'NONE', 'NONE', #16528,  #16217 ) ;
#8179 = LINE ( 'NONE', #14080, #16759 ) ;
#8180 = DIRECTION ( 'NONE',  ( 4.675871521838985949E-16, -1.000000000000000000, -0.000000000000000000 ) ) ;
#8181 = ORIENTED_EDGE ( 'NONE', *, *, #2539, .T. ) ;
#8182 = DIRECTION ( 'NONE',  ( -0.000000000000000000, -0.000000000000000000, 1.000000000000000000 ) ) ;
#8183 = FACE_OUTER_BOUND ( 'NONE', #1887, .T. ) ;
#8184 = CARTESIAN_POINT ( 'NONE',  ( -70.71978124295668522, -96.08423613455721579, -28.18308811886538479 ) ) ;
#8185 = ORIENTED_EDGE ( 'NONE', *, *, #8363, .T. ) ;
#8186 = AXIS2_PLACEMENT_3D ( 'NONE', #6361, #6458, #10592 ) ;
#8187 = CARTESIAN_POINT ( 'NONE',  ( -75.91366687898980103, 106.7636614011200891, -27.61062523460392981 ) ) ;
#8188 = DIRECTION ( 'NONE',  ( 0.000000000000000000, 5.551115123125747573E-17, 1.000000000000000000 ) ) ;
#8190 = ORIENTED_EDGE ( 'NONE', *, *, #17104, .T. ) ;
#8189 = EDGE_CURVE ( 'NONE', #3765, #11369, #7850, .T. ) ;
#8191 = FACE_OUTER_BOUND ( 'NONE', #14525, .T. ) ;
#8192 = EDGE_CURVE ( 'NONE', #18188, #10024, #12561, .T. ) ;
#8193 = DIRECTION ( 'NONE',  ( 0.000000000000000000, 1.000000000000000000, 0.000000000000000000 ) ) ;
#8194 = ORIENTED_EDGE ( 'NONE', *, *, #8775, .F. ) ;
#8195 = AXIS2_PLACEMENT_3D ( 'NONE', #9788, #18488, #6983 ) ;
#8196 = CIRCLE ( 'NONE', #9748, 34.36884788726141693 ) ;
#8197 = VECTOR ( 'NONE', #2472, 1000.000000000000114 ) ;
#8198 = CIRCLE ( 'NONE', #14758, 85.91469608272775815 ) ;
#8199 = ORIENTED_EDGE ( 'NONE', *, *, #17595, .T. ) ;
#8200 = CARTESIAN_POINT ( 'NONE',  ( -67.59262256747315689, 111.6514400295689313, -15.00000000000001066 ) ) ;
#8201 = EDGE_LOOP ( 'NONE', ( #4854, #6123, #735, #16880, #12907, #2335 ) ) ;
#8202 = CARTESIAN_POINT ( 'NONE',  ( 49.38736944425944841, -141.5628872026273086, -57.00000000000000000 ) ) ;
#8203 = DIRECTION ( 'NONE',  ( -0.000000000000000000, -0.000000000000000000, 1.000000000000000000 ) ) ;
#8204 = FACE_OUTER_BOUND ( 'NONE', #13611, .T. ) ;
#8205 = FACE_OUTER_BOUND ( 'NONE', #16973, .T. ) ;
#8206 = ORIENTED_EDGE ( 'NONE', *, *, #12829, .F. ) ;
#8207 = COLOUR_RGB ( '',0.7921568627450980005, 0.8196078431372548767, 0.9333333333333333481 ) ;
#8208 = DIRECTION ( 'NONE',  ( 0.000000000000000000, 1.000000000000000000, 0.000000000000000000 ) ) ;
#8209 = DIRECTION ( 'NONE',  ( 1.156482317317869999E-16, 0.000000000000000000, 1.000000000000000000 ) ) ;
#8210 = LINE ( 'NONE', #8010, #464 ) ;
#8211 = CARTESIAN_POINT ( 'NONE',  ( -21.28916685891738325, 36.54437923629615170, -35.57537618398750823 ) ) ;
#8212 = DIRECTION ( 'NONE',  ( -0.9396926207859084279, 0.3420201433256686574, 0.000000000000000000 ) ) ;
#8213 = ORIENTED_EDGE ( 'NONE', *, *, #600, .T. ) ;
#8214 = CIRCLE ( 'NONE', #7912, 4.600000000000006750 ) ;
#8215 = CIRCLE ( 'NONE', #1073, 12.49999999999999645 ) ;
#8216 = AXIS2_PLACEMENT_3D ( 'NONE', #18458, #14147, #5623 ) ;
#8217 = FACE_OUTER_BOUND ( 'NONE', #9982, .T. ) ;
#8218 = CARTESIAN_POINT ( 'NONE',  ( -64.80066835027112404, -94.42547236494611695, 44.74948972093436339 ) ) ;
#8219 = DIRECTION ( 'NONE',  ( 4.675871521838985949E-16, -1.000000000000000000, -0.000000000000000000 ) ) ;
#8220 = SURFACE_SIDE_STYLE ('',( #18037 ) ) ;
#8221 = ORIENTED_EDGE ( 'NONE', *, *, #6400, .F. ) ;
#8222 = ORIENTED_EDGE ( 'NONE', *, *, #15334, .T. ) ;
#8223 = EDGE_CURVE ( 'NONE', #2867, #11561, #17700, .T. ) ;
#8224 = CARTESIAN_POINT ( 'NONE',  ( -92.59262256747318531, 0.3328663868096687350, 25.00000000000000000 ) ) ;
#8225 = VECTOR ( 'NONE', #12418, 1000.000000000000000 ) ;
#8226 = ORIENTED_EDGE ( 'NONE', *, *, #4222, .F. ) ;
#8227 = AXIS2_PLACEMENT_3D ( 'NONE', #11947, #10451, #3337 ) ;
#8228 = VECTOR ( 'NONE', #9227, 1000.000000000000000 ) ;
#8229 = LINE ( 'NONE', #14032, #15981 ) ;
#8230 = LINE ( 'NONE', #2709, #16820 ) ;
#8231 = PLANE ( 'NONE',  #12059 ) ;
#8232 = ORIENTED_EDGE ( 'NONE', *, *, #4450, .T. ) ;
#8233 = DIRECTION ( 'NONE',  ( 0.000000000000000000, 1.000000000000000000, 0.000000000000000000 ) ) ;
#8234 = CARTESIAN_POINT ( 'NONE',  ( -67.59262256747315689, 129.5689604715732912, -15.00000000000001066 ) ) ;
#8235 = CARTESIAN_POINT ( 'NONE',  ( -68.99615306438094819, 55.41708673813027985, -15.00000000000001421 ) ) ;
#8236 = CARTESIAN_POINT ( 'NONE',  ( -56.80760832784252301, 71.73152654333280509, -15.00000000000001421 ) ) ;
#8237 = ORIENTED_EDGE ( 'NONE', *, *, #4310, .F. ) ;
#8238 = EDGE_CURVE ( 'NONE', #12144, #4238, #3940, .T. ) ;
#8239 = EDGE_CURVE ( 'NONE', #2148, #17871, #6840, .T. ) ;
#8240 = FACE_OUTER_BOUND ( 'NONE', #7631, .T. ) ;
#8241 = DIRECTION ( 'NONE',  ( -0.9396926207859171987, 0.3420201433256444545, 1.086737899652999999E-16 ) ) ;
#8242 = ORIENTED_EDGE ( 'NONE', *, *, #7449, .F. ) ;
#8243 = FACE_OUTER_BOUND ( 'NONE', #18005, .T. ) ;
#8244 = AXIS2_PLACEMENT_3D ( 'NONE', #10828, #4939, #13729 ) ;
#8245 = LINE ( 'NONE', #12368, #7139 ) ;
#8247 = ORIENTED_EDGE ( 'NONE', *, *, #5033, .F. ) ;
#8246 = VECTOR ( 'NONE', #14923, 1000.000000000000114 ) ;
#8248 = ORIENTED_EDGE ( 'NONE', *, *, #1188, .T. ) ;
#8249 = ADVANCED_FACE ( 'NONE', ( #7193 ), #2639, .T. ) ;
#8250 = EDGE_CURVE ( 'NONE', #14911, #9679, #4850, .T. ) ;
#8251 = ORIENTED_EDGE ( 'NONE', *, *, #1969, .T. ) ;
#8252 = PLANE ( 'NONE',  #4030 ) ;
#8253 = DIRECTION ( 'NONE',  ( -1.000000000000000000, -2.062304371594500494E-16, -0.000000000000000000 ) ) ;
#8254 = CARTESIAN_POINT ( 'NONE',  ( -68.99615306438097662, 61.08541618166268705, -15.00000000000001421 ) ) ;
#8255 = CARTESIAN_POINT ( 'NONE',  ( -66.63376473465912397, -19.34983604512935429, -3.000000000000000000 ) ) ;
#8256 = EDGE_CURVE ( 'NONE', #11278, #3670, #12913, .T. ) ;
#8257 = LINE ( 'NONE', #8628, #8361 ) ;
#8258 = DIRECTION ( 'NONE',  ( 0.000000000000000000, 1.000000000000000000, 0.000000000000000000 ) ) ;
#8259 = ORIENTED_EDGE ( 'NONE', *, *, #14956, .T. ) ;
#8260 = ADVANCED_FACE ( 'NONE', ( #13963 ), #18261, .T. ) ;
#8261 = CARTESIAN_POINT ( 'NONE',  ( -67.59262256747319952, 111.6514400295689171, 22.50837044127971254 ) ) ;
#8262 = DIRECTION ( 'NONE',  ( 1.000000000000000000, 2.062304371594500740E-16, 0.000000000000000000 ) ) ;
#8264 = ORIENTED_EDGE ( 'NONE', *, *, #11575, .T. ) ;
#8263 = CARTESIAN_POINT ( 'NONE',  ( 5.233202738124664855, -111.0842361345572158, 57.00000000000000000 ) ) ;
#8265 = DIRECTION ( 'NONE',  ( -0.000000000000000000, 0.000000000000000000, 1.000000000000000000 ) ) ;
#8266 = EDGE_CURVE ( 'NONE', #9970, #15423, #8154, .T. ) ;
#8267 = ADVANCED_FACE ( 'NONE', ( #16744 ), #5252, .T. ) ;
#8268 = DIRECTION ( 'NONE',  ( -1.000000000000000000, -0.000000000000000000, -0.000000000000000000 ) ) ;
#8269 = ORIENTED_EDGE ( 'NONE', *, *, #9149, .T. ) ;
#8270 = LINE ( 'NONE', #9473, #9496 ) ;
#8271 = VERTEX_POINT ( 'NONE', #17203 ) ;
#8272 = EDGE_CURVE ( 'NONE', #9327, #8420, #4387, .T. ) ;
#8273 = ORIENTED_EDGE ( 'NONE', *, *, #12939, .T. ) ;
#8274 = CARTESIAN_POINT ( 'NONE',  ( -53.39175999306721110, 74.07097899412303832, -15.00000000000001421 ) ) ;
#8275 = DIRECTION ( 'NONE',  ( 1.000000000000000000, 0.000000000000000000, 0.000000000000000000 ) ) ;
#8276 = CARTESIAN_POINT ( 'NONE',  ( -71.24615306438093398, 66.54966845456371516, -15.00000000000001421 ) ) ;
#8277 = VERTEX_POINT ( 'NONE', #13770 ) ;
#8278 = PRODUCT_CONTEXT ( 'NONE', #9803, 'mechanical' ) ;
#8279 = EDGE_LOOP ( 'NONE', ( #15535, #12035, #2203, #14104 ) ) ;
#8280 = CARTESIAN_POINT ( 'NONE',  ( 15.23320273812466219, -15.06406080364910771, -54.10850799397452704 ) ) ;
#8281 = CARTESIAN_POINT ( 'NONE',  ( -71.24615306438070661, 134.7758360152292312, -167.1454815528550739 ) ) ;
#8282 = ORIENTED_EDGE ( 'NONE', *, *, #4989, .T. ) ;
#8283 = DIRECTION ( 'NONE',  ( -5.204170427930409450E-16, 0.000000000000000000, 1.000000000000000000 ) ) ;
#8284 = CARTESIAN_POINT ( 'NONE',  ( -92.59262256747319952, 57.88796029049330372, -30.35917033480640370 ) ) ;
#8285 = CARTESIAN_POINT ( 'NONE',  ( 95.45835937779679625, 56.41207303426869402, 7.000000000000010658 ) ) ;
#8286 = ORIENTED_EDGE ( 'NONE', *, *, #6780, .F. ) ;
#8287 = LINE ( 'NONE', #18296, #1194 ) ;
#8288 = LINE ( 'NONE', #11092, #2464 ) ;
#8289 = ORIENTED_EDGE ( 'NONE', *, *, #7062, .F. ) ;
#8290 = CARTESIAN_POINT ( 'NONE',  ( -64.09025127992791226, 117.8748711238780373, -7.000000000000013323 ) ) ;
#8291 = VERTEX_POINT ( 'NONE', #9759 ) ;
#8292 = ORIENTED_EDGE ( 'NONE', *, *, #14508, .F. ) ;
#8293 = CARTESIAN_POINT ( 'NONE',  ( -68.99615306438093398, 71.12504998813029999, -15.00000000000001421 ) ) ;
#8294 = DIRECTION ( 'NONE',  ( 0.000000000000000000, -5.551115123125747573E-17, -1.000000000000000000 ) ) ;
#8295 = ORIENTED_EDGE ( 'NONE', *, *, #3090, .F. ) ;
#8296 = CARTESIAN_POINT ( 'NONE',  ( -107.5926225674731711, 65.58224449241410525, 20.00000000000000355 ) ) ;
#8297 = DIRECTION ( 'NONE',  ( -1.000000000000000000, 3.330669073875471988E-15, 1.387778780781446662E-16 ) ) ;
#8298 = CARTESIAN_POINT ( 'NONE',  ( -78.23321842955243710, 73.26749283226919829, 102.5000000000000000 ) ) ;
#8299 = CARTESIAN_POINT ( 'NONE',  ( -65.72457281170906640, 78.72276507608454210, -15.00000000000001421 ) ) ;
#8300 = ORIENTED_EDGE ( 'NONE', *, *, #4266, .T. ) ;
#8301 = DIRECTION ( 'NONE',  ( 0.000000000000000000, 1.000000000000000000, 0.000000000000000000 ) ) ;
#8302 = DIRECTION ( 'NONE',  ( 0.000000000000000000, 1.000000000000000000, 0.000000000000000000 ) ) ;
#8303 = CARTESIAN_POINT ( 'NONE',  ( -24.41997999089026550, 38.95069813737347886, -34.21586952458824982 ) ) ;
#8304 = CARTESIAN_POINT ( 'NONE',  ( 3.080246995596566340, 23.75572429475707636, 41.96082232098843434 ) ) ;
#8305 = EDGE_LOOP ( 'NONE', ( #6965, #15966, #9908, #8607, #12174 ) ) ;
#8306 = CYLINDRICAL_SURFACE ( 'NONE', #1051, 12.49999999999999112 ) ;
#8307 = DIRECTION ( 'NONE',  ( 1.000000000000000000, 0.000000000000000000, 0.000000000000000000 ) ) ;
#8308 = DIRECTION ( 'NONE',  ( 0.000000000000000000, 0.000000000000000000, -1.000000000000000000 ) ) ;
#8309 = DIRECTION ( 'NONE',  ( -0.9396926207859068736, 0.3420201433256726542, 1.086737899652988043E-16 ) ) ;
#8310 = ORIENTED_EDGE ( 'NONE', *, *, #6117, .F. ) ;
#8311 = VERTEX_POINT ( 'NONE', #14392 ) ;
#8312 = PRODUCT_RELATED_PRODUCT_CATEGORY ( 'part', '', ( #13410 ) ) ;
#8314 = EDGE_CURVE ( 'NONE', #8559, #794, #12277, .T. ) ;
#8313 = CARTESIAN_POINT ( 'NONE',  ( -71.24615306438084872, 101.1071876045637055, -15.00000000000001421 ) ) ;
#8315 = ORIENTED_EDGE ( 'NONE', *, *, #14291, .T. ) ;
#8316 = LINE ( 'NONE', #17009, #15082 ) ;
#8317 = LINE ( 'NONE', #9529, #1588 ) ;
#8318 = CIRCLE ( 'NONE', #2942, 3.999999999999982681 ) ;
#8319 = DIRECTION ( 'NONE',  ( 0.000000000000000000, 0.000000000000000000, 1.000000000000000000 ) ) ;
#8320 = ORIENTED_EDGE ( 'NONE', *, *, #10923, .T. ) ;
#8321 = CARTESIAN_POINT ( 'NONE',  ( -66.26485270048019061, 109.8219421365140249, -28.00000000000000000 ) ) ;
#8322 = FACE_OUTER_BOUND ( 'NONE', #5066, .T. ) ;
#8323 = CARTESIAN_POINT ( 'NONE',  ( -68.99615306438091977, 77.40823528813029952, 15.00000000000006928 ) ) ;
#8324 = EDGE_LOOP ( 'NONE', ( #16142, #14046, #1455, #4664 ) ) ;
#8325 = ADVANCED_FACE ( 'NONE', ( #5153 ), #15157, .F. ) ;
#8326 = DIRECTION ( 'NONE',  ( 0.000000000000000000, 0.000000000000000000, 1.000000000000000000 ) ) ;
#8327 = ORIENTED_EDGE ( 'NONE', *, *, #11685, .F. ) ;
#8328 = FACE_OUTER_BOUND ( 'NONE', #9364, .T. ) ;
#8329 = B_SPLINE_CURVE_WITH_KNOTS ( 'NONE', 3,
 ( #9866, #8280, #2858, #13898, #13990, #18103, #16771, #8369, #16672, #5460, #2759, #5356, #8465, #1263, #1445, #9776, #1170, #14176, #11370, #7069, #6779, #9680, #6868, #5558, #4158, #15390, #12781, #2579 ),
 .UNSPECIFIED., .F., .F.,
 ( 4, 2, 2, 2, 2, 2, 2, 2, 2, 2, 2, 2, 2, 4 ),
 ( 0.000000000000000000, 0.01281839044724412263, 0.02563678089448824526, 0.02884137850629928113, 0.03204597611811031699, 0.03845517134173238177, 0.05127356178897649747, 0.05768275701259856225, 0.06409195223622063398, 0.07691034268346474967, 0.08331953790708679364, 0.08652413551889782950, 0.08972873313070885148, 0.1025471235779529533 ),
 .UNSPECIFIED. ) ;
#8330 = DIRECTION ( 'NONE',  ( 0.000000000000000000, 0.000000000000000000, 1.000000000000000000 ) ) ;
#8331 = ORIENTED_EDGE ( 'NONE', *, *, #18075, .F. ) ;
#8332 = CIRCLE ( 'NONE', #13399, 10.24900000000001477 ) ;
#8333 = ORIENTED_EDGE ( 'NONE', *, *, #2621, .F. ) ;
#8334 = EDGE_CURVE ( 'NONE', #15321, #4520, #15317, .T. ) ;
#8335 = ORIENTED_EDGE ( 'NONE', *, *, #8719, .T. ) ;
#8336 = PRODUCT_DEFINITION_CONTEXT ( 'detailed design', #8853, 'design' ) ;
#8337 = EDGE_CURVE ( 'NONE', #16250, #13337, #5871, .T. ) ;
#8338 = CARTESIAN_POINT ( 'NONE',  ( -69.25739799065789271, 57.48797571754649738, -22.35917033480642502 ) ) ;
#8339 = PLANE ( 'NONE',  #9357 ) ;
#8340 = DIRECTION ( 'NONE',  ( 0.000000000000000000, 5.551115123125748189E-17, 1.000000000000000000 ) ) ;
#8341 = CARTESIAN_POINT ( 'NONE',  ( -57.08002265617300708, 84.22855780814606419, -35.00000000000000000 ) ) ;
#8342 = DIRECTION ( 'NONE',  ( 0.000000000000000000, 1.000000000000000000, 0.000000000000000000 ) ) ;
#8343 = FACE_OUTER_BOUND ( 'NONE', #1940, .T. ) ;
#8344 = ORIENTED_EDGE ( 'NONE', *, *, #2054, .F. ) ;
#8345 = VECTOR ( 'NONE', #1818, 1000.000000000000000 ) ;
#8346 = EDGE_CURVE ( 'NONE', #11711, #197, #6048, .T. ) ;
#8347 = LINE ( 'NONE', #8631, #15876 ) ;
#8348 = ORIENTED_EDGE ( 'NONE', *, *, #17719, .F. ) ;
#8349 = EDGE_CURVE ( 'NONE', #4147, #16002, #1872, .T. ) ;
#8350 = CARTESIAN_POINT ( 'NONE',  ( 95.45835937779679625, 56.41207303426869402, 3.000000000000000000 ) ) ;
#8351 = CARTESIAN_POINT ( 'NONE',  ( -68.99615306438083451, 99.39938383813029077, 15.00000000000006928 ) ) ;
#8352 = ORIENTED_EDGE ( 'NONE', *, *, #16945, .F. ) ;
#8353 = DIRECTION ( 'NONE',  ( -1.000000000000000000, -0.000000000000000000, -0.000000000000000000 ) ) ;
#8354 = ORIENTED_EDGE ( 'NONE', *, *, #8360, .F. ) ;
#8355 = PRODUCT_DEFINITION_SHAPE ( 'NONE', 'NONE',  #15399 ) ;
#8356 = EDGE_CURVE ( 'NONE', #573, #18453, #1750, .T. ) ;
#8358 = EDGE_CURVE ( 'NONE', #2873, #11376, #9055, .T. ) ;
#8357 = CONICAL_SURFACE ( 'NONE', #283, 6.500000000000039968, 1.047197551196600296 ) ;
#8359 = ORIENTED_EDGE ( 'NONE', *, *, #10867, .T. ) ;
#8360 = EDGE_CURVE ( 'NONE', #6937, #11248, #3330, .T. ) ;
#8361 = VECTOR ( 'NONE', #6943, 1000.000000000000000 ) ;
#8362 = FILL_AREA_STYLE_COLOUR ( '', #151 ) ;
#8363 = EDGE_CURVE ( 'NONE', #6958, #15269, #7286, .T. ) ;
#8364 = CARTESIAN_POINT ( 'NONE',  ( -40.83486628351231218, 66.64375664990294013, 102.5000000000000000 ) ) ;
#8365 = DIRECTION ( 'NONE',  ( -5.204170427930409450E-16, 0.000000000000000000, 1.000000000000000000 ) ) ;
#8366 = ORIENTED_EDGE ( 'NONE', *, *, #15471, .F. ) ;
#8367 = ITEM_DEFINED_TRANSFORMATION ( 'NONE', 'NONE', #18016,  #16217 ) ;
#8368 = ORIENTED_EDGE ( 'NONE', *, *, #116, .F. ) ;
#8369 = CARTESIAN_POINT ( 'NONE',  ( 10.09019014590969654, 9.228091135629581387, -47.65272416155497837 ) ) ;
#8370 = DIRECTION ( 'NONE',  ( -0.000000000000000000, -0.000000000000000000, -1.000000000000000000 ) ) ;
#8371 = ORIENTED_EDGE ( 'NONE', *, *, #6268, .F. ) ;
#8372 = EDGE_CURVE ( 'NONE', #3309, #12209, #10545, .T. ) ;
#8373 = FACE_OUTER_BOUND ( 'NONE', #15153, .T. ) ;
#8374 = EDGE_CURVE ( 'NONE', #15261, #14168, #9350, .T. ) ;
#8375 = FACE_OUTER_BOUND ( 'NONE', #13627, .T. ) ;
#8376 = EDGE_CURVE ( 'NONE', #13839, #14227, #7551, .T. ) ;
#8377 = VERTEX_POINT ( 'NONE', #16240 ) ;
#8378 = VECTOR ( 'NONE', #10783, 1000.000000000000000 ) ;
#8379 = DIRECTION ( 'NONE',  ( 0.000000000000000000, 1.000000000000000000, 0.000000000000000000 ) ) ;
#8380 = DIRECTION ( 'NONE',  ( 0.000000000000000000, 1.000000000000000000, 0.000000000000000000 ) ) ;
#8381 = ORIENTED_EDGE ( 'NONE', *, *, #17445, .F. ) ;
#8382 = CIRCLE ( 'NONE', #8680, 34.36884788726143114 ) ;
#8383 = CARTESIAN_POINT ( 'NONE',  ( -68.99615306438100504, 39.09426763166271002, 15.00000000000006928 ) ) ;
#8384 = CARTESIAN_POINT ( 'NONE',  ( -100.4870060002411805, -151.5628872026273086, -18.23991632971910803 ) ) ;
#8385 = ORIENTED_EDGE ( 'NONE', *, *, #5835, .T. ) ;
#8386 = CIRCLE ( 'NONE', #14361, 10.38004356723770627 ) ;
#8387 = ADVANCED_FACE ( 'NONE', ( #8876 ), #17280, .T. ) ;
#8388 = DIRECTION ( 'NONE',  ( -0.7071067811865496822, 4.734329415645505418E-17, -0.7071067811865453523 ) ) ;
#8389 = CIRCLE ( 'NONE', #3006, 3.999999999999996447 ) ;
#8390 = EDGE_CURVE ( 'NONE', #5168, #9316, #14743, .T. ) ;
#8391 = PLANE ( 'NONE',  #13553 ) ;
#8392 = EDGE_LOOP ( 'NONE', ( #14782, #15002, #9104, #743 ) ) ;
#8393 = AXIS2_PLACEMENT_3D ( 'NONE', #16994, #9710, #11018 ) ;
#8394 = DIRECTION ( 'NONE',  ( 0.000000000000000000, 0.000000000000000000, 1.000000000000000000 ) ) ;
#8395 = CARTESIAN_POINT ( 'NONE',  ( -54.78701292294434211, 94.21775734381050427, 15.00000000000006928 ) ) ;
#8396 = VECTOR ( 'NONE', #9437, 1000.000000000000000 ) ;
#8397 = LINE ( 'NONE', #15303, #104 ) ;
#8398 = DIRECTION ( 'NONE',  ( 1.000000000000000000, 0.000000000000000000, 0.000000000000000000 ) ) ;
#8399 = VERTEX_POINT ( 'NONE', #3428 ) ;
#8400 = CARTESIAN_POINT ( 'NONE',  ( -71.24615306438082030, 97.96559495456375544, -15.00000000000001421 ) ) ;
#8401 = FACE_OUTER_BOUND ( 'NONE', #12541, .T. ) ;
#8402 = DIRECTION ( 'NONE',  ( -1.000000000000000000, 3.016910393003138520E-15, 0.000000000000000000 ) ) ;
#8403 = FACE_OUTER_BOUND ( 'NONE', #9265, .T. ) ;
#8404 = VERTEX_POINT ( 'NONE', #1575 ) ;
#8405 = CIRCLE ( 'NONE', #17046, 12.49999999999999112 ) ;
#8406 = DIRECTION ( 'NONE',  ( 1.000000000000000000, 0.000000000000000000, 0.000000000000000000 ) ) ;
#8407 = CARTESIAN_POINT ( 'NONE',  ( -71.24615306438097662, 63.40807580456375803, -167.1454815528550739 ) ) ;
#8408 = VECTOR ( 'NONE', #17098, 1000.000000000000000 ) ;
#8409 = CARTESIAN_POINT ( 'NONE',  ( -64.58002265617299997, 84.22855780814606419, 35.00000000000000000 ) ) ;
#8410 = AXIS2_PLACEMENT_3D ( 'NONE', #10622, #6197, #11923 ) ;
#8411 = DIRECTION ( 'NONE',  ( 1.000000000000000000, 0.000000000000000000, 5.551115123125784674E-16 ) ) ;
#8412 = ORIENTED_EDGE ( 'NONE', *, *, #5722, .F. ) ;
#8413 = ORIENTED_EDGE ( 'NONE', *, *, #6020, .T. ) ;
#8414 = CARTESIAN_POINT ( 'NONE',  ( -57.08002265617300708, 84.22855780814606419, 37.50000000000000000 ) ) ;
#8415 = MECHANICAL_DESIGN_GEOMETRIC_PRESENTATION_REPRESENTATION (  '', ( #8709 ), #2738 ) ;
#8416 = VERTEX_POINT ( 'NONE', #3165 ) ;
#8417 = CARTESIAN_POINT ( 'NONE',  ( -97.59262256747317110, 0.3328663868096687350, 25.00000000000000000 ) ) ;
#8418 = DIRECTION ( 'NONE',  ( 0.000000000000000000, -0.000000000000000000, -1.000000000000000000 ) ) ;
#8419 = CARTESIAN_POINT ( 'NONE',  ( -63.40980125876012607, -92.35432432510548040, -43.13417342538324561 ) ) ;
#8420 = VERTEX_POINT ( 'NONE', #13007 ) ;
#8421 = DIRECTION ( 'NONE',  ( 1.000000000000000000, 0.000000000000000000, 5.551115123125777772E-16 ) ) ;
#8422 = CIRCLE ( 'NONE', #337, 29.36884788726140627 ) ;
#8423 = DIRECTION ( 'NONE',  ( 0.000000000000000000, 0.000000000000000000, 1.000000000000000000 ) ) ;
#8424 = DIRECTION ( 'NONE',  ( 0.000000000000000000, 0.8660254037844375974, -0.5000000000000017764 ) ) ;
#8425 = CARTESIAN_POINT ( 'NONE',  ( -79.12361985383350316, 84.22855780814606419, -61.50000000000000000 ) ) ;
#8426 = VERTEX_POINT ( 'NONE', #8962 ) ;
#8427 = DIRECTION ( 'NONE',  ( -0.000000000000000000, -0.000000000000000000, 1.000000000000000000 ) ) ;
#8428 = ORIENTED_EDGE ( 'NONE', *, *, #8594, .T. ) ;
#8429 = EDGE_CURVE ( 'NONE', #9931, #7647, #13090, .T. ) ;
#8430 = AXIS2_PLACEMENT_3D ( 'NONE', #11267, #10038, #5894 ) ;
#8431 = PLANE ( 'NONE',  #12577 ) ;
#8432 = DIRECTION ( 'NONE',  ( -0.000000000000000000, -1.000000000000000000, -0.000000000000000000 ) ) ;
#8433 = ORIENTED_EDGE ( 'NONE', *, *, #815, .T. ) ;
#8434 = ORIENTED_EDGE ( 'NONE', *, *, #10037, .F. ) ;
#8435 = VECTOR ( 'NONE', #16222, 1000.000000000000000 ) ;
#8436 = CIRCLE ( 'NONE', #5428, 4.025000000000000355 ) ;
#8437 = VERTEX_POINT ( 'NONE', #14569 ) ;
#8438 = PLANE ( 'NONE',  #8216 ) ;
#8439 = DIRECTION ( 'NONE',  ( -0.9396926207859092051, 0.3420201433256663259, 0.000000000000000000 ) ) ;
#8440 = CARTESIAN_POINT ( 'NONE',  ( -64.22944241949029731, 91.57211267264378307, 15.00000000000006928 ) ) ;
#8441 = VECTOR ( 'NONE', #11494, 1000.000000000000000 ) ;
#8442 = LINE ( 'NONE', #12562, #13436 ) ;
#8443 = CARTESIAN_POINT ( 'NONE',  ( -91.19225650277898865, 92.96220022626712876, 92.50000000000000000 ) ) ;
#8444 = ORIENTED_EDGE ( 'NONE', *, *, #5526, .F. ) ;
#8445 = FACE_OUTER_BOUND ( 'NONE', #1545, .T. ) ;
#8446 = ORIENTED_EDGE ( 'NONE', *, *, #16130, .F. ) ;
#8447 = CARTESIAN_POINT ( 'NONE',  ( 0.000000000000000000, 0.000000000000000000, 3.000000000000000000 ) ) ;
#8448 = VECTOR ( 'NONE', #2373, 1000.000000000000000 ) ;
#8449 = CIRCLE ( 'NONE', #6319, 85.91469608272775815 ) ;
#8450 = CARTESIAN_POINT ( 'NONE',  ( -68.99615306438094819, 70.51019413166270056, -167.1454815528550739 ) ) ;
#8451 = EDGE_LOOP ( 'NONE', ( #3092, #7081, #17446, #16943, #15658, #12771 ) ) ;
#8452 = EDGE_CURVE ( 'NONE', #10991, #8271, #7456, .T. ) ;
#8453 = CARTESIAN_POINT ( 'NONE',  ( -113.2720846013048543, -91.96846159163189327, -7.798230460770719574 ) ) ;
#8454 = VERTEX_POINT ( 'NONE', #6038 ) ;
#8455 = AXIS2_PLACEMENT_3D ( 'NONE', #18099, #15475, #11277 ) ;
#8456 = ORIENTED_EDGE ( 'NONE', *, *, #16606, .F. ) ;
#8457 = ADVANCED_FACE ( 'NONE', ( #11767 ), #444, .T. ) ;
#8458 = VECTOR ( 'NONE', #9837, 1000.000000000000114 ) ;
#8459 = AXIS2_PLACEMENT_3D ( 'NONE', #8184, #11472, #11375 ) ;
#8460 = DIRECTION ( 'NONE',  ( 0.000000000000000000, 1.000000000000000000, 0.000000000000000000 ) ) ;
#8461 = CARTESIAN_POINT ( 'NONE',  ( 15.23320273812466041, -19.34983604512935429, 57.00000000000000000 ) ) ;
#8462 = DIRECTION ( 'NONE',  ( 1.000000000000000000, 0.000000000000000000, 0.000000000000000000 ) ) ;
#8463 = ORIENTED_EDGE ( 'NONE', *, *, #15789, .F. ) ;
#8464 = VERTEX_POINT ( 'NONE', #14657 ) ;
#8465 = CARTESIAN_POINT ( 'NONE',  ( 3.062581012969010974, 23.78654787968694961, -41.94750742838608915 ) ) ;
#8466 = CARTESIAN_POINT ( 'NONE',  ( -33.72855994630469212, 78.95224028009285178, 92.50000000000000000 ) ) ;
#8467 = EDGE_LOOP ( 'NONE', ( #5213, #15776, #7922, #11417, #3037, #6854 ) ) ;
#8468 = AXIS2_PLACEMENT_3D ( 'NONE', #17462, #4649, #10363 ) ;
#8469 = DIRECTION ( 'NONE',  ( 0.9915318908039647550, 1.590368294782254281E-17, 0.1298634264091108326 ) ) ;
#8470 = CYLINDRICAL_SURFACE ( 'NONE', #6593, 10.24900000000000055 ) ;
#8471 = CARTESIAN_POINT ( 'NONE',  ( -49.26569365422058411, 90.86016871721223254, -167.1454815528550739 ) ) ;
#8472 = EDGE_LOOP ( 'NONE', ( #5223, #16778, #998, #9687, #11073 ) ) ;
#8473 = ADVANCED_FACE ( 'NONE', ( #17543 ), #8097, .F. ) ;
#8474 = PLANE ( 'NONE',  #11360 ) ;
#8475 = DIRECTION ( 'NONE',  ( 1.156482317317869999E-16, 0.000000000000000000, 1.000000000000000000 ) ) ;
#8476 = VERTEX_POINT ( 'NONE', #3605 ) ;
#8477 = EDGE_CURVE ( 'NONE', #14981, #11552, #12341, .T. ) ;
#8478 = VECTOR ( 'NONE', #8809, 1000.000000000000114 ) ;
#8479 = VECTOR ( 'NONE', #5895, 1000.000000000000000 ) ;
#8480 = DIRECTION ( 'NONE',  ( 0.000000000000000000, 0.000000000000000000, -1.000000000000000000 ) ) ;
#8482 = ORIENTED_EDGE ( 'NONE', *, *, #717, .T. ) ;
#8481 = AXIS2_PLACEMENT_3D ( 'NONE', #16716, #12537, #18235 ) ;
#8483 = CARTESIAN_POINT ( 'NONE',  ( -71.24615306438076345, 125.3510580652292248, -167.1454815528550739 ) ) ;
#8484 = ORIENTED_EDGE ( 'NONE', *, *, #7873, .F. ) ;
#8485 = VERTEX_POINT ( 'NONE', #7824 ) ;
#8486 = EDGE_CURVE ( 'NONE', #2327, #10261, #3892, .T. ) ;
#8487 = EDGE_CURVE ( 'NONE', #13457, #8085, #2023, .T. ) ;
#8488 = EDGE_CURVE ( 'NONE', #15333, #14280, #13440, .T. ) ;
#8489 = FACE_OUTER_BOUND ( 'NONE', #5291, .T. ) ;
#8490 = CARTESIAN_POINT ( 'NONE',  ( 56.85086857400936822, 84.22855780814606419, 55.00000000000000711 ) ) ;
#8491 = ORIENTED_EDGE ( 'NONE', *, *, #5273, .T. ) ;
#8492 = EDGE_CURVE ( 'NONE', #773, #16082, #5203, .T. ) ;
#8493 = PRODUCT_DEFINITION_FORMATION_WITH_SPECIFIED_SOURCE ( 'ANY', '', #2679, .NOT_KNOWN. ) ;
#8494 = VECTOR ( 'NONE', #15493, 1000.000000000000000 ) ;
#8495 = CARTESIAN_POINT ( 'NONE',  ( -68.99615306438091977, 73.65178678166269322, 15.00000000000006928 ) ) ;
#8497 = VECTOR ( 'NONE', #6596, 1000.000000000000000 ) ;
#8496 = CARTESIAN_POINT ( 'NONE',  ( -68.99615306438086293, 93.11619853813030545, 15.00000000000006928 ) ) ;
#8498 = LINE ( 'NONE', #18497, #5772 ) ;
#8499 = DIRECTION ( 'NONE',  ( 1.000000000000000000, 0.000000000000000000, 0.000000000000000000 ) ) ;
#8500 = VERTEX_POINT ( 'NONE', #9507 ) ;
#8501 = EDGE_CURVE ( 'NONE', #11612, #8311, #10818, .T. ) ;
#8502 = LINE ( 'NONE', #2394, #14069 ) ;
#8503 =( REPRESENTATION_RELATIONSHIP ('NONE','NONE', #359, #5501 ) REPRESENTATION_RELATIONSHIP_WITH_TRANSFORMATION ( #17239 )SHAPE_REPRESENTATION_RELATIONSHIP( ) );
#8504 = CARTESIAN_POINT ( 'NONE',  ( -29.49754210169703939, 42.18689076489602741, -32.29756042961390960 ) ) ;
#8505 = DIRECTION ( 'NONE',  ( 0.3420201433256456203, 0.9396926207859168656, -0.000000000000000000 ) ) ;
#8506 = EDGE_LOOP ( 'NONE', ( #3113, #13277, #2711, #5296 ) ) ;
#8507 = EDGE_CURVE ( 'NONE', #9948, #1399, #18021, .T. ) ;
#8508 = CARTESIAN_POINT ( 'NONE',  ( -68.99615306438077766, 124.5321250381302747, -167.1454815528550739 ) ) ;
#8509 = DIRECTION ( 'NONE',  ( 0.000000000000000000, 1.000000000000000000, 0.000000000000000000 ) ) ;
#8510 = EDGE_CURVE ( 'NONE', #1656, #1289, #2117, .T. ) ;
#8511 = CARTESIAN_POINT ( 'NONE',  ( -123.4618227840623632, -111.0842361345572158, 7.000000000000013323 ) ) ;
#8512 = VECTOR ( 'NONE', #1555, 1000.000000000000000 ) ;
#8513 = CARTESIAN_POINT ( 'NONE',  ( -57.08002265617300708, 84.22855780814606419, -167.1454815528550739 ) ) ;
#8514 = ORIENTED_EDGE ( 'NONE', *, *, #10844, .F. ) ;
#8515 = AXIS2_PLACEMENT_3D ( 'NONE', #10680, #9099, #7778 ) ;
#8516 = ORIENTED_EDGE ( 'NONE', *, *, #7436, .T. ) ;
#8517 = EDGE_CURVE ( 'NONE', #7155, #16713, #5299, .T. ) ;
#8518 = CYLINDRICAL_SURFACE ( 'NONE', #12364, 26.04359719766049253 ) ;
#8519 = AXIS2_PLACEMENT_3D ( 'NONE', #1439, #13890, #1085 ) ;
#8520 = ORIENTED_EDGE ( 'NONE', *, *, #15457, .T. ) ;
#8521 = CARTESIAN_POINT ( 'NONE',  ( -66.71236600666622962, 111.9737865874585481, -24.23198523837357143 ) ) ;
#8522 = CARTESIAN_POINT ( 'NONE',  ( -75.31304609867017064, 61.20467279731714427, 24.11916851373873882 ) ) ;
#8523 = FACE_BOUND ( 'NONE', #321, .T. ) ;
#8524 = VERTEX_POINT ( 'NONE', #13816 ) ;
#8525 = AXIS2_PLACEMENT_3D ( 'NONE', #5658, #9882, #1099 ) ;
#8526 = CARTESIAN_POINT ( 'NONE',  ( -64.09025127992788384, 50.58224449241410525, 35.00000000000000000 ) ) ;
#8527 = CIRCLE ( 'NONE', #12406, 4.599999999999992539 ) ;
#8528 = CARTESIAN_POINT ( 'NONE',  ( -68.99615306438111872, 10.81993378166265529, -15.00000000000001421 ) ) ;
#8529 = LINE ( 'NONE', #17208, #1083 ) ;
#8530 = VECTOR ( 'NONE', #6751, 1000.000000000000000 ) ;
#8531 = DIRECTION ( 'NONE',  ( 0.000000000000000000, 0.000000000000000000, 1.000000000000000000 ) ) ;
#8532 = EDGE_LOOP ( 'NONE', ( #516, #467, #16941, #14641, #10830 ) ) ;
#8533 = PLANE ( 'NONE',  #8983 ) ;
#8534 = ORIENTED_EDGE ( 'NONE', *, *, #1285, .F. ) ;
#8535 = CARTESIAN_POINT ( 'NONE',  ( -71.24615306438073503, 128.4926507152292459, -167.1454815528550739 ) ) ;
#8536 = FILL_AREA_STYLE ('',( #15638 ) ) ;
#8537 = VERTEX_POINT ( 'NONE', #9325 ) ;
#8538 = ORIENTED_EDGE ( 'NONE', *, *, #8132, .T. ) ;
#8539 = AXIS2_PLACEMENT_3D ( 'NONE', #4004, #15424, #6809 ) ;
#8540 = VECTOR ( 'NONE', #5692, 1000.000000000000000 ) ;
#8541 = AXIS2_PLACEMENT_3D ( 'NONE', #16832, #6633, #9736 ) ;
#8542 = ORIENTED_EDGE ( 'NONE', *, *, #7926, .F. ) ;
#8543 = FACE_OUTER_BOUND ( 'NONE', #364, .T. ) ;
#8544 = FACE_OUTER_BOUND ( 'NONE', #15729, .T. ) ;
#8545 = CARTESIAN_POINT ( 'NONE',  ( -78.12361985383348895, 83.72858089318386021, 70.00000000000002842 ) ) ;
#8546 = DIRECTION ( 'NONE',  ( 0.000000000000000000, 0.000000000000000000, 1.000000000000000000 ) ) ;
#8547 = CARTESIAN_POINT ( 'NONE',  ( -65.06546592763129411, -111.0842361345572158, -6.816485587782003001E-13 ) ) ;
#8548 = ORIENTED_EDGE ( 'NONE', *, *, #14867, .F. ) ;
#8549 = DIRECTION ( 'NONE',  ( 0.000000000000000000, 0.000000000000000000, 1.000000000000000000 ) ) ;
#8551 = ADVANCED_FACE ( 'NONE', ( #1006 ), #6314, .T. ) ;
#8550 = ORIENTED_EDGE ( 'NONE', *, *, #14091, .F. ) ;
#8552 = CARTESIAN_POINT ( 'NONE',  ( -71.24615306438067819, 145.0894847045637732, 15.00000000000006928 ) ) ;
#8553 = AXIS2_PLACEMENT_3D ( 'NONE', #18130, #16703, #11218 ) ;
#8554 = AXIS2_PLACEMENT_3D ( 'NONE', #3897, #12524, #9605 ) ;
#8555 = LINE ( 'NONE', #18468, #13431 ) ;
#8556 = VERTEX_POINT ( 'NONE', #12327 ) ;
#8557 = CARTESIAN_POINT ( 'NONE',  ( -112.9698934257354352, -91.80660034481556409, -8.049308492552277983 ) ) ;
#8558 = ORIENTED_EDGE ( 'NONE', *, *, #226, .F. ) ;
#8559 = VERTEX_POINT ( 'NONE', #16326 ) ;
#8560 = CARTESIAN_POINT ( 'NONE',  ( 95.45835937779682467, 4.463510241361116170E-14, -3.000000000000000000 ) ) ;
#8561 = CARTESIAN_POINT ( 'NONE',  ( -65.06546592763139358, -111.0842361345572158, 28.18308811886540610 ) ) ;
#8562 = ORIENTED_EDGE ( 'NONE', *, *, #12728, .T. ) ;
#8563 = LINE ( 'NONE', #18287, #14382 ) ;
#8564 = PLANE ( 'NONE',  #3433 ) ;
#8565 = ORIENTED_EDGE ( 'NONE', *, *, #6255, .F. ) ;
#8566 = LINE ( 'NONE', #5561, #7492 ) ;
#8567 = CARTESIAN_POINT ( 'NONE',  ( 0.5805565836007747782, -7.505553499465293932, 1.040834085586084257E-14 ) ) ;
#8568 = FACE_OUTER_BOUND ( 'NONE', #10164, .T. ) ;
#8569 = VERTEX_POINT ( 'NONE', #16697 ) ;
#8570 = CARTESIAN_POINT ( 'NONE',  ( 79.02261728059691848, -151.5628872026273086, 57.00000000000000000 ) ) ;
#8571 = ORIENTED_EDGE ( 'NONE', *, *, #1076, .F. ) ;
#8572 = EDGE_CURVE ( 'NONE', #10176, #8070, #5006, .T. ) ;
#8573 = ORIENTED_EDGE ( 'NONE', *, *, #366, .T. ) ;
#8574 = LINE ( 'NONE', #15404, #136 ) ;
#8575 = ORIENTED_EDGE ( 'NONE', *, *, #18428, .T. ) ;
#8576 = FACE_OUTER_BOUND ( 'NONE', #7639, .T. ) ;
#8577 = EDGE_CURVE ( 'NONE', #8399, #7810, #17743, .T. ) ;
#8578 = DIRECTION ( 'NONE',  ( 0.000000000000000000, -0.5000000000000017764, -0.8660254037844377084 ) ) ;
#8579 = DIRECTION ( 'NONE',  ( -1.000000000000000000, 0.000000000000000000, 0.000000000000000000 ) ) ;
#8580 = ORIENTED_EDGE ( 'NONE', *, *, #952, .F. ) ;
#8581 = PLANE ( 'NONE',  #17024 ) ;
#8582 = LINE ( 'NONE', #14287, #4170 ) ;
#8583 = CARTESIAN_POINT ( 'NONE',  ( -71.24615306438097662, 56.23601976522923707, -15.00000000000001421 ) ) ;
#8584 = CARTESIAN_POINT ( 'NONE',  ( -68.99615306438120399, -1.746436818337276931, -167.1454815528550739 ) ) ;
#8585 = ORIENTED_EDGE ( 'NONE', *, *, #11454, .F. ) ;
#8586 = DIRECTION ( 'NONE',  ( 0.000000000000000000, 1.000000000000000000, 0.000000000000000000 ) ) ;
#8587 = DIRECTION ( 'NONE',  ( -1.000000000000000000, 0.000000000000000000, 0.000000000000000000 ) ) ;
#8588 = FACE_OUTER_BOUND ( 'NONE', #2649, .T. ) ;
#8589 = ORIENTED_EDGE ( 'NONE', *, *, #2652, .T. ) ;
#8590 = EDGE_CURVE ( 'NONE', #2581, #6749, #11270, .T. ) ;
#8591 = EDGE_CURVE ( 'NONE', #12513, #1656, #3981, .T. ) ;
#8592 = CARTESIAN_POINT ( 'NONE',  ( -58.95655619609375009, 74.15281352429524020, 15.00000000000006928 ) ) ;
#8593 = CARTESIAN_POINT ( 'NONE',  ( -71.24615306438089135, 81.36876096522922808, -15.00000000000001421 ) ) ;
#8594 = EDGE_CURVE ( 'NONE', #1045, #7123, #15336, .T. ) ;
#8595 = CARTESIAN_POINT ( 'NONE',  ( -44.49764538373973721, 84.22855780814606419, 25.00000000000000355 ) ) ;
#8596 = LINE ( 'NONE', #11229, #23 ) ;
#8597 = VERTEX_POINT ( 'NONE', #8583 ) ;
#8598 = VERTEX_POINT ( 'NONE', #2685 ) ;
#8599 = EDGE_CURVE ( 'NONE', #13376, #8923, #2789, .T. ) ;
#8600 = EDGE_CURVE ( 'NONE', #5572, #16527, #8498, .T. ) ;
#8601 = CARTESIAN_POINT ( 'NONE',  ( -64.09025127992788384, 50.58224449241410525, 35.00000000000000000 ) ) ;
#8602 = ORIENTED_EDGE ( 'NONE', *, *, #2385, .T. ) ;
#8603 = ADVANCED_FACE ( 'NONE', ( #9600 ), #11468, .T. ) ;
#8604 = CARTESIAN_POINT ( 'NONE',  ( -68.76426085488260753, 88.67024416760638417, 15.00000000000006928 ) ) ;
#8605 = EDGE_CURVE ( 'NONE', #10059, #5963, #6670, .T. ) ;
#8606 = PLANE ( 'NONE',  #14464 ) ;
#8607 = ORIENTED_EDGE ( 'NONE', *, *, #14235, .F. ) ;
#8608 = DIRECTION ( 'NONE',  ( 0.9396926207859084279, 0.3420201433256686574, 4.890320548438448905E-16 ) ) ;
#8609 = CARTESIAN_POINT ( 'NONE',  ( -68.99615306438089135, 67.36860148166267948, -167.1454815528550739 ) ) ;
#8610 = CARTESIAN_POINT ( 'NONE',  ( -38.40244272411881354, 55.35140561506842261, 23.53852893732882379 ) ) ;
#8611 = CARTESIAN_POINT ( 'NONE',  ( 0.2595206531158220642, 2.531175536751704147, 6.499999999999982236 ) ) ;
#8612 = ORIENTED_EDGE ( 'NONE', *, *, #3795, .F. ) ;
#8613 = DIRECTION ( 'NONE',  ( -0.9396926207859022107, 0.3420201433256853663, 1.086737899652982620E-16 ) ) ;
#8614 = EDGE_CURVE ( 'NONE', #18335, #14903, #16209, .T. ) ;
#8615 = EDGE_CURVE ( 'NONE', #6278, #2307, #8397, .T. ) ;
#8616 = LINE ( 'NONE', #5527, #7478 ) ;
#8617 = ORIENTED_EDGE ( 'NONE', *, *, #1525, .F. ) ;
#8618 = DIRECTION ( 'NONE',  ( 1.156482317317869999E-16, 0.000000000000000000, 1.000000000000000000 ) ) ;
#8619 = LINE ( 'NONE', #10109, #316 ) ;
#8620 = ORIENTED_EDGE ( 'NONE', *, *, #18213, .F. ) ;
#8621 = ORIENTED_EDGE ( 'NONE', *, *, #3608, .F. ) ;
#8622 = AXIS2_PLACEMENT_3D ( 'NONE', #2847, #15920, #17142 ) ;
#8623 = SHAPE_REPRESENTATION ( 'Axle Retaining Ring', ( #16217 ), #8171 ) ;
#8624 = DIRECTION ( 'NONE',  ( -0.000000000000000000, -0.000000000000000000, -1.000000000000000000 ) ) ;
#8625 = CARTESIAN_POINT ( 'NONE',  ( -71.24615306438087714, 82.25763170456374951, -15.00000000000001421 ) ) ;
#8626 = EDGE_CURVE ( 'NONE', #409, #10136, #17087, .T. ) ;
#8627 = DIRECTION ( 'NONE',  ( 0.000000000000000000, 0.000000000000000000, 1.000000000000000000 ) ) ;
#8628 = CARTESIAN_POINT ( 'NONE',  ( -68.99615306438070661, 136.4836397816626743, -15.00000000000001421 ) ) ;
#8629 = LINE ( 'NONE', #12846, #10497 ) ;
#8630 = ORIENTED_EDGE ( 'NONE', *, *, #12433, .F. ) ;
#8631 = CARTESIAN_POINT ( 'NONE',  ( -68.99615306438103346, 33.42593818813029571, -167.1454815528550739 ) ) ;
#8632 = ORIENTED_EDGE ( 'NONE', *, *, #17911, .F. ) ;
#8633 = CARTESIAN_POINT ( 'NONE',  ( -76.37409655828278687, -95.65021661331557823, 45.05044770573179846 ) ) ;
#8634 = DIRECTION ( 'NONE',  ( -1.000000000000000000, 3.016910393003138520E-15, 0.000000000000000000 ) ) ;
#8635 = AXIS2_PLACEMENT_3D ( 'NONE', #3835, #5327, #16843 ) ;
#8636 = ORIENTED_EDGE ( 'NONE', *, *, #13387, .F. ) ;
#8637 = FACE_OUTER_BOUND ( 'NONE', #14875, .T. ) ;
#8638 = ORIENTED_EDGE ( 'NONE', *, *, #687, .F. ) ;
#8639 = EDGE_LOOP ( 'NONE', ( #7103, #15672, #824, #12774 ) ) ;
#8640 = CARTESIAN_POINT ( 'NONE',  ( -59.20641439073742873, 73.63336328296978195, 15.00000000000006928 ) ) ;
#8641 = AXIS2_PLACEMENT_3D ( 'NONE', #13030, #17390, #5711 ) ;
#8642 = DIRECTION ( 'NONE',  ( -1.000000000000000000, 2.220446049250309925E-14, 1.387778780781443703E-16 ) ) ;
#8643 = CARTESIAN_POINT ( 'NONE',  ( -67.59262256747315689, 117.8748711238780373, -15.00000000000001066 ) ) ;
#8644 = EDGE_LOOP ( 'NONE', ( #1443, #8264, #6620, #9226 ) ) ;
#8645 = DIRECTION ( 'NONE',  ( -0.000000000000000000, -0.000000000000000000, -1.000000000000000000 ) ) ;
#8646 = VERTEX_POINT ( 'NONE', #1293 ) ;
#8647 = CARTESIAN_POINT ( 'NONE',  ( -71.24615306438074924, 104.2487802545637692, 15.00000000000006928 ) ) ;
#8648 = DIRECTION ( 'NONE',  ( 1.000000000000000000, 2.062304371594500494E-16, 0.000000000000000000 ) ) ;
#8649 = DIRECTION ( 'NONE',  ( 1.156482317317869999E-16, 0.000000000000000000, 1.000000000000000000 ) ) ;
#8650 = VERTEX_POINT ( 'NONE', #12799 ) ;
#8651 = DIRECTION ( 'NONE',  ( 0.000000000000000000, 0.000000000000000000, -1.000000000000000000 ) ) ;
#8652 = ORIENTED_EDGE ( 'NONE', *, *, #11095, .T. ) ;
#8653 = VERTEX_POINT ( 'NONE', #8298 ) ;
#8654 = AXIS2_PLACEMENT_3D ( 'NONE', #12190, #16383, #10607 ) ;
#8655 = ADVANCED_FACE ( 'NONE', ( #18414 ), #11302, .T. ) ;
#8656 = CARTESIAN_POINT ( 'NONE',  ( -68.99615306438111872, 11.43478963813029914, 15.00000000000006928 ) ) ;
#8657 = AXIS2_PLACEMENT_3D ( 'NONE', #4177, #18018, #16900 ) ;
#8658 = EDGE_LOOP ( 'NONE', ( #6231, #17721, #14811, #16303 ) ) ;
#8659 = ORIENTED_EDGE ( 'NONE', *, *, #10884, .T. ) ;
#8660 = CARTESIAN_POINT ( 'NONE',  ( -57.08002265617300708, 84.22855780814606419, -62.50000000000000000 ) ) ;
#8661 = ORIENTED_EDGE ( 'NONE', *, *, #907, .F. ) ;
#8662 = CARTESIAN_POINT ( 'NONE',  ( -67.44681693414594292, 91.21279551874751235, -15.00000000000001243 ) ) ;
#8663 = CARTESIAN_POINT ( 'NONE',  ( -92.59262256747321373, 114.3311569208253786, -25.00000000000000000 ) ) ;
#8664 = CARTESIAN_POINT ( 'NONE',  ( -71.24615306438089135, 81.36876096522922808, -167.1454815528550739 ) ) ;
#8665 = VECTOR ( 'NONE', #16756, 1000.000000000000114 ) ;
#8666 = DIRECTION ( 'NONE',  ( 0.000000000000000000, 1.000000000000000000, 0.000000000000000000 ) ) ;
#8667 = ORIENTED_EDGE ( 'NONE', *, *, #6637, .F. ) ;
#8668 = CARTESIAN_POINT ( 'NONE',  ( -64.58002265617299997, 84.22855780814606419, -35.00000000000000000 ) ) ;
#8669 = AXIS2_PLACEMENT_3D ( 'NONE', #7431, #11991, #10597 ) ;
#8670 = DIRECTION ( 'NONE',  ( 0.000000000000000000, 1.000000000000000000, 0.000000000000000000 ) ) ;
#8671 = CARTESIAN_POINT ( 'NONE',  ( -71.24615306438099083, 38.27533460456378123, 15.00000000000006928 ) ) ;
#8672 = ORIENTED_EDGE ( 'NONE', *, *, #8942, .T. ) ;
#8673 = CARTESIAN_POINT ( 'NONE',  ( -81.37409655828275845, -91.08423613455721579, 28.18308811886534571 ) ) ;
#8674 = EDGE_CURVE ( 'NONE', #6741, #2018, #17183, .T. ) ;
#8675 = DIRECTION ( 'NONE',  ( 0.000000000000000000, 1.000000000000000000, 0.000000000000000000 ) ) ;
#8676 = LINE ( 'NONE', #76, #15555 ) ;
#8677 = ORIENTED_EDGE ( 'NONE', *, *, #15664, .F. ) ;
#8678 = AXIS2_PLACEMENT_3D ( 'NONE', #1495, #17212, #2991 ) ;
#8679 = ORIENTED_EDGE ( 'NONE', *, *, #5146, .T. ) ;
#8680 = AXIS2_PLACEMENT_3D ( 'NONE', #5035, #16540, #2047 ) ;
#8681 = CIRCLE ( 'NONE', #6894, 3.999999999999989786 ) ;
#8682 = DIRECTION ( 'NONE',  ( 1.000000000000000000, 0.000000000000000000, 0.000000000000000000 ) ) ;
#8683 = ADVANCED_FACE ( 'NONE', ( #8204 ), #4279, .T. ) ;
#8684 = DIRECTION ( 'NONE',  ( 0.000000000000000000, 0.7787792746743906758, -0.6272980482494985299 ) ) ;
#8685 = CARTESIAN_POINT ( 'NONE',  ( -66.22475908702843128, 112.1374203547857036, -25.60634877502412721 ) ) ;
#8686 = PLANE ( 'NONE',  #11749 ) ;
#8687 = DIRECTION ( 'NONE',  ( 0.3420201433256481738, -0.9396926207859158664, 0.000000000000000000 ) ) ;
#8688 = DIRECTION ( 'NONE',  ( 0.000000000000000000, 1.000000000000000000, 0.000000000000000000 ) ) ;
#8689 = ADVANCED_FACE ( 'NONE', ( #9706 ), #1193, .T. ) ;
#8690 = EDGE_LOOP ( 'NONE', ( #15526, #7318, #11840, #6087 ) ) ;
#8691 =( GEOMETRIC_REPRESENTATION_CONTEXT ( 3 ) GLOBAL_UNCERTAINTY_ASSIGNED_CONTEXT ( ( #13957 ) ) GLOBAL_UNIT_ASSIGNED_CONTEXT ( ( #368, #6330, #7839 ) ) REPRESENTATION_CONTEXT ( 'NONE', 'WORKASPACE' ) );
#8692 = LINE ( 'NONE', #13178, #10754 ) ;
#8693 = PLANE ( 'NONE',  #1658 ) ;
#8694 = DIRECTION ( 'NONE',  ( 2.062304371594500494E-16, -1.000000000000000000, 0.000000000000000000 ) ) ;
#8695 = DIRECTION ( 'NONE',  ( -1.000000000000000000, -0.000000000000000000, -0.000000000000000000 ) ) ;
#8696 = ORIENTED_EDGE ( 'NONE', *, *, #17385, .T. ) ;
#8697 = AXIS2_PLACEMENT_3D ( 'NONE', #2329, #2536, #16840 ) ;
#8698 = DIRECTION ( 'NONE',  ( -1.000000000000000000, 0.000000000000000000, 0.000000000000000000 ) ) ;
#8700 = ADVANCED_FACE ( 'NONE', ( #1819 ), #4707, .T. ) ;
#8699 = VECTOR ( 'NONE', #3896, 1000.000000000000227 ) ;
#8701 = LINE ( 'NONE', #17118, #11070 ) ;
#8702 = EDGE_CURVE ( 'NONE', #13724, #2315, #10426, .T. ) ;
#8703 = VERTEX_POINT ( 'NONE', #11919 ) ;
#8704 = EDGE_CURVE ( 'NONE', #4718, #7872, #9302, .T. ) ;
#8705 = CARTESIAN_POINT ( 'NONE',  ( -171.0109138863553824, 84.22855780814606419, 70.00000000000001421 ) ) ;
#8706 = CARTESIAN_POINT ( 'NONE',  ( -68.94671286412481948, 88.15687341518439268, 15.00000000000006928 ) ) ;
#8707 = EDGE_LOOP ( 'NONE', ( #16599, #8385, #135, #1684 ) ) ;
#8708 = VERTEX_POINT ( 'NONE', #8939 ) ;
#8709=STYLED_ITEM('',(#18545),#6489);
#8710 = EDGE_CURVE ( 'NONE', #2059, #2407, #1917, .T. ) ;
#8711 = ORIENTED_EDGE ( 'NONE', *, *, #12727, .F. ) ;
#8712 = EDGE_CURVE ( 'NONE', #15993, #8797, #3225, .T. ) ;
#8713 = AXIS2_PLACEMENT_3D ( 'NONE', #18480, #11374, #11470 ) ;
#8714 = EDGE_CURVE ( 'NONE', #5859, #9827, #16118, .T. ) ;
#8715 = VECTOR ( 'NONE', #3663, 1000.000000000000000 ) ;
#8716 = LINE ( 'NONE', #14418, #1637 ) ;
#8717 = CARTESIAN_POINT ( 'NONE',  ( 0.2578475836321327264, -4.367703157927462776, 5.434916218090863893 ) ) ;
#8718 = CARTESIAN_POINT ( 'NONE',  ( -59.05157857372951469, 96.57209730311865314, -167.1454815528550739 ) ) ;
#8719 = EDGE_CURVE ( 'NONE', #8972, #9420, #10200, .T. ) ;
#8720 = DIRECTION ( 'NONE',  ( 0.000000000000000000, 0.000000000000000000, 1.000000000000000000 ) ) ;
#8721 = PLANE ( 'NONE',  #14674 ) ;
#8722 = ORIENTED_EDGE ( 'NONE', *, *, #8775, .T. ) ;
#8723 = ADVANCED_FACE ( 'NONE', ( #3307 ), #9030, .T. ) ;
#8724 = DIRECTION ( 'NONE',  ( 1.000000000000000000, 0.000000000000000000, 0.000000000000000000 ) ) ;
#8725 = ORIENTED_EDGE ( 'NONE', *, *, #4933, .T. ) ;
#8726 = AXIS2_PLACEMENT_3D ( 'NONE', #1518, #15546, #11539 ) ;
#8727 = CARTESIAN_POINT ( 'NONE',  ( -107.5926225674732137, 117.8748711238780373, -25.00000000000000000 ) ) ;
#8728 = CARTESIAN_POINT ( 'NONE',  ( -67.50540723371459251, 87.07303407725210320, -15.00000000000001421 ) ) ;
#8729 = ORIENTED_EDGE ( 'NONE', *, *, #13086, .F. ) ;
#8730 = VECTOR ( 'NONE', #9333, 1000.000000000000000 ) ;
#8731 = AXIS2_PLACEMENT_3D ( 'NONE', #4751, #6242, #476 ) ;
#8732 = CARTESIAN_POINT ( 'NONE',  ( -98.90286936182235422, -96.08423613455721579, -2.027180301682503564E-13 ) ) ;
#8733 = EDGE_CURVE ( 'NONE', #5426, #16629, #8422, .T. ) ;
#8734 = ADVANCED_FACE ( 'NONE', ( #324 ), #423, .T. ) ;
#8735 = EDGE_LOOP ( 'NONE', ( #12133, #3488, #16447, #4719 ) ) ;
#8736 = AXIS2_PLACEMENT_3D ( 'NONE', #17899, #3502, #2008 ) ;
#8737 = CARTESIAN_POINT ( 'NONE',  ( -67.59262256747315689, 56.80567558672318285, 37.50000000000000000 ) ) ;
#8738 = APPLICATION_CONTEXT ( 'automotive_design' ) ;
#8739 = LINE ( 'NONE', #3120, #422 ) ;
#8740 = FACE_OUTER_BOUND ( 'NONE', #1088, .T. ) ;
#8741 = VERTEX_POINT ( 'NONE', #10152 ) ;
#8742 = CIRCLE ( 'NONE', #16488, 4.599999999999999645 ) ;
#8743 = AXIS2_PLACEMENT_3D ( 'NONE', #8968, #17470, #4655 ) ;
#8744 = ORIENTED_EDGE ( 'NONE', *, *, #11258, .F. ) ;
#8745 = CARTESIAN_POINT ( 'NONE',  ( -93.54007869656273044, 187.7866419848965052, 15.00000000000006928 ) ) ;
#8746 = FACE_BOUND ( 'NONE', #641, .T. ) ;
#8747 = DIRECTION ( 'NONE',  ( 0.000000000000000000, 1.000000000000000000, 0.000000000000000000 ) ) ;
#8748 = DIRECTION ( 'NONE',  ( -0.000000000000000000, -0.000000000000000000, 1.000000000000000000 ) ) ;
#8749 = ORIENTED_EDGE ( 'NONE', *, *, #5699, .F. ) ;
#8750 = CARTESIAN_POINT ( 'NONE',  ( -50.90853507983961634, 93.09943318379598054, -167.1454815528550739 ) ) ;
#8751 = ORIENTED_EDGE ( 'NONE', *, *, #17610, .F. ) ;
#8752 = AXIS2_PLACEMENT_3D ( 'NONE', #3864, #9571, #13892 ) ;
#8753 = VERTEX_POINT ( 'NONE', #15953 ) ;
#8754 = AXIS2_PLACEMENT_3D ( 'NONE', #15155, #4965, #11985 ) ;
#8755 = AXIS2_PLACEMENT_3D ( 'NONE', #13403, #582, #9381 ) ;
#8756 = EDGE_LOOP ( 'NONE', ( #3966, #4250, #10711, #14692 ) ) ;
#8757 = CARTESIAN_POINT ( 'NONE',  ( 0.000000000000000000, 0.000000000000000000, 35.00000000000000000 ) ) ;
#8758 = DIRECTION ( 'NONE',  ( -0.000000000000000000, -0.000000000000000000, -1.000000000000000000 ) ) ;
#8759 = CARTESIAN_POINT ( 'NONE',  ( -71.24615306438111872, 19.42577870456376132, -15.00000000000001421 ) ) ;
#8760 = VECTOR ( 'NONE', #17969, 1000.000000000000114 ) ;
#8761 = ORIENTED_EDGE ( 'NONE', *, *, #1943, .T. ) ;
#8762 = LINE ( 'NONE', #14465, #10738 ) ;
#8763 = LINE ( 'NONE', #10425, #5042 ) ;
#8764 = CARTESIAN_POINT ( 'NONE',  ( -68.99615306438111872, 7.678341131662685726, 15.00000000000006928 ) ) ;
#8765 = LINE ( 'NONE', #7363, #1635 ) ;
#8766 = ORIENTED_EDGE ( 'NONE', *, *, #1968, .T. ) ;
#8767 = EDGE_CURVE ( 'NONE', #3371, #9665, #509, .T. ) ;
#8768 = LINE ( 'NONE', #4534, #14086 ) ;
#8769 = AXIS2_PLACEMENT_3D ( 'NONE', #5513, #6916, #16924 ) ;
#8770 = VECTOR ( 'NONE', #6850, 1000.000000000000000 ) ;
#8771 = AXIS2_PLACEMENT_3D ( 'NONE', #11317, #1481, #13937 ) ;
#8772 = CARTESIAN_POINT ( 'NONE',  ( 4.699999999999995737, 5.629165124598801917, 3.250000000000037748 ) ) ;
#8773 = PLANE ( 'NONE',  #12642 ) ;
#8774 = ORIENTED_EDGE ( 'NONE', *, *, #7750, .T. ) ;
#8775 = EDGE_CURVE ( 'NONE', #3955, #4742, #5928, .T. ) ;
#8776 = CARTESIAN_POINT ( 'NONE',  ( -66.96222586426215173, 88.60139997190893268, 15.00000000000006928 ) ) ;
#8777 = LINE ( 'NONE', #3235, #4743 ) ;
#8778 = ORIENTED_EDGE ( 'NONE', *, *, #8429, .F. ) ;
#8779 = ORIENTED_EDGE ( 'NONE', *, *, #2509, .T. ) ;
#8780 = AXIS2_PLACEMENT_3D ( 'NONE', #999, #9887, #8579 ) ;
#8781 = CIRCLE ( 'NONE', #12684, 4.000000000000024869 ) ;
#8782 = DIRECTION ( 'NONE',  ( 0.000000000000000000, 0.000000000000000000, 1.000000000000000000 ) ) ;
#8783 = DIRECTION ( 'NONE',  ( 0.000000000000000000, 0.000000000000000000, 1.000000000000000000 ) ) ;
#8784 = DIRECTION ( 'NONE',  ( 1.156482317317869999E-16, 0.000000000000000000, 1.000000000000000000 ) ) ;
#8785 = PLANE ( 'NONE',  #4599 ) ;
#8786 = ORIENTED_EDGE ( 'NONE', *, *, #4562, .F. ) ;
#8787 = COLOUR_RGB ( '',0.7921568627450980005, 0.8196078431372548767, 0.9333333333333333481 ) ;
#8788 = CARTESIAN_POINT ( 'NONE',  ( 4.699999999999995737, -7.505553499465293932, 1.040834085586084257E-14 ) ) ;
#8789 = DIRECTION ( 'NONE',  ( 0.000000000000000000, 0.000000000000000000, -1.000000000000000000 ) ) ;
#8790 = FACE_OUTER_BOUND ( 'NONE', #8467, .T. ) ;
#8791 = DIRECTION ( 'NONE',  ( -0.7071067811865496822, 3.925231146709400939E-17, 0.7071067811865453523 ) ) ;
#8792 = ORIENTED_EDGE ( 'NONE', *, *, #13221, .F. ) ;
#8793 = CARTESIAN_POINT ( 'NONE',  ( -37.39908167440526654, 91.67867170800822407, 63.49367417844965900 ) ) ;
#8794 = VECTOR ( 'NONE', #15121, 1000.000000000000000 ) ;
#8795 = CIRCLE ( 'NONE', #3117, 12.50000000000000355 ) ;
#8796 = FACE_OUTER_BOUND ( 'NONE', #8756, .T. ) ;
#8797 = VERTEX_POINT ( 'NONE', #7264 ) ;
#8798 = EDGE_CURVE ( 'NONE', #10024, #18464, #17342, .T. ) ;
#8799 = LINE ( 'NONE', #5964, #3012 ) ;
#8800 = DIRECTION ( 'NONE',  ( -0.004825104377941397994, -0.9999883591161159435, -2.511066551536017787E-18 ) ) ;
#8801 = ORIENTED_EDGE ( 'NONE', *, *, #8108, .T. ) ;
#8802 = ORIENTED_EDGE ( 'NONE', *, *, #16810, .T. ) ;
#8803 = MECHANICAL_DESIGN_GEOMETRIC_PRESENTATION_REPRESENTATION (  '', ( #1046 ), #17447 ) ;
#8804 = VECTOR ( 'NONE', #16425, 1000.000000000000000 ) ;
#8805 = ORIENTED_EDGE ( 'NONE', *, *, #18102, .T. ) ;
#8806 = CIRCLE ( 'NONE', #4331, 3.999999999999989786 ) ;
#8807 = CIRCLE ( 'NONE', #4333, 10.24899999999998812 ) ;
#8808 = CARTESIAN_POINT ( 'NONE',  ( -65.17806329749801364, 93.75072866207683830, 15.00000000000006928 ) ) ;
#8809 = DIRECTION ( 'NONE',  ( 0.9396926207859084279, 0.3420201433256686574, -1.086737899652989892E-16 ) ) ;
#8810 = EDGE_CURVE ( 'NONE', #16126, #4629, #3148, .T. ) ;
#8811 = DIRECTION ( 'NONE',  ( 0.000000000000000000, 0.000000000000000000, 1.000000000000000000 ) ) ;
#8812 = ADVANCED_FACE ( 'NONE', ( #8859 ), #3048, .T. ) ;
#8813 = CARTESIAN_POINT ( 'NONE',  ( -76.37409655828275845, -111.0842361345572158, 28.18308811886536347 ) ) ;
#8814 = PLANE ( 'NONE',  #17081 ) ;
#8815 = ORIENTED_EDGE ( 'NONE', *, *, #11893, .T. ) ;
#8816 = CIRCLE ( 'NONE', #5529, 10.24900000000000766 ) ;
#8817 = CARTESIAN_POINT ( 'NONE',  ( 4.699999999999995737, 3.752776749732559924, -6.500000000000061284 ) ) ;
#8818 = DIRECTION ( 'NONE',  ( -1.000000000000000000, 0.000000000000000000, 0.000000000000000000 ) ) ;
#8819 = CARTESIAN_POINT ( 'NONE',  ( -71.24615306438109030, 28.85055665456373575, 15.00000000000006928 ) ) ;
#8820 = VERTEX_POINT ( 'NONE', #1731 ) ;
#8821 = AXIS2_PLACEMENT_3D ( 'NONE', #14188, #6790, #8480 ) ;
#8822 = EDGE_CURVE ( 'NONE', #2315, #14578, #7433, .T. ) ;
#8823 = ADVANCED_FACE ( 'NONE', ( #2364 ), #6577, .F. ) ;
#8824 = DIRECTION ( 'NONE',  ( 0.9396926207859069846, 0.3420201433256723766, 4.890320548438442003E-16 ) ) ;
#8825 = TOROIDAL_SURFACE ( 'NONE', #155, 2.168074330098863189, 5.000000000000000000 ) ;
#8826 = DIRECTION ( 'NONE',  ( -1.000000000000000000, 0.000000000000000000, 0.000000000000000000 ) ) ;
#8828 = ORIENTED_EDGE ( 'NONE', *, *, #10411, .T. ) ;
#8827 = CIRCLE ( 'NONE', #13308, 5.654315315325682434 ) ;
#8829 = ORIENTED_EDGE ( 'NONE', *, *, #7552, .T. ) ;
#8830 = EDGE_CURVE ( 'NONE', #18243, #5195, #4800, .T. ) ;
#8831 = LINE ( 'NONE', #5824, #5206 ) ;
#8832 = EDGE_CURVE ( 'NONE', #2924, #13982, #3616, .T. ) ;
#8833 = DIRECTION ( 'NONE',  ( 0.000000000000000000, 1.000000000000000000, 0.000000000000000000 ) ) ;
#8834 = DIRECTION ( 'NONE',  ( 0.000000000000000000, 1.000000000000000000, 0.000000000000000000 ) ) ;
#8835 = AXIS2_PLACEMENT_3D ( 'NONE', #2484, #8086, #9493 ) ;
#8836 = ORIENTED_EDGE ( 'NONE', *, *, #18428, .F. ) ;
#8837 = AXIS2_PLACEMENT_3D ( 'NONE', #2123, #13181, #13546 ) ;
#8838 = EDGE_CURVE ( 'NONE', #2538, #881, #3690, .T. ) ;
#8839 = AXIS2_PLACEMENT_3D ( 'NONE', #2395, #5303, #2304 ) ;
#8840 = LINE ( 'NONE', #7602, #8715 ) ;
#8841 = EDGE_CURVE ( 'NONE', #3501, #2330, #17807, .T. ) ;
#8842 = EDGE_LOOP ( 'NONE', ( #3624, #8562, #13103, #2707 ) ) ;
#8843 = CYLINDRICAL_SURFACE ( 'NONE', #9901, 5.000000000000004441 ) ;
#8844 = DIRECTION ( 'NONE',  ( 0.000000000000000000, -0.000000000000000000, -1.000000000000000000 ) ) ;
#8845 = CARTESIAN_POINT ( 'NONE',  ( -71.24615306438089135, 84.51035361522924916, 15.00000000000006928 ) ) ;
#8846 = DIRECTION ( 'NONE',  ( -0.9396926207859097602, 0.3420201433256649381, -4.890320548438455808E-16 ) ) ;
#8847 = ORIENTED_EDGE ( 'NONE', *, *, #2041, .F. ) ;
#8848 = DIRECTION ( 'NONE',  ( -0.000000000000000000, -0.000000000000000000, -1.000000000000000000 ) ) ;
#8849 = VERTEX_POINT ( 'NONE', #6390 ) ;
#8850 = ADVANCED_FACE ( 'NONE', ( #14815 ), #16308, .F. ) ;
#8851 = ORIENTED_EDGE ( 'NONE', *, *, #4689, .T. ) ;
#8852 = CIRCLE ( 'NONE', #17790, 12.49999999999999112 ) ;
#8853 = APPLICATION_CONTEXT ( 'automotive_design' ) ;
#8854 = DIRECTION ( 'NONE',  ( 0.000000000000000000, 0.000000000000000000, -1.000000000000000000 ) ) ;
#8855 = CARTESIAN_POINT ( 'NONE',  ( -123.4618227840623632, 84.22855780814606419, 62.50000000000001421 ) ) ;
#8856 = EDGE_LOOP ( 'NONE', ( #614, #16845, #9417, #13974 ) ) ;
#8857 = CARTESIAN_POINT ( 'NONE',  ( -49.97371631896665178, 107.0896764944441202, 92.50000000000000000 ) ) ;
#8858 = DIRECTION ( 'NONE',  ( 0.000000000000000000, 1.000000000000000000, 0.000000000000000000 ) ) ;
#8859 = FACE_OUTER_BOUND ( 'NONE', #16519, .T. ) ;
#8860 = CARTESIAN_POINT ( 'NONE',  ( -76.37409655828265898, -91.08423613455721579, -2.461913000519969422E-13 ) ) ;
#8861 = ORIENTED_EDGE ( 'NONE', *, *, #14754, .T. ) ;
#8862 = CARTESIAN_POINT ( 'NONE',  ( -61.60537251683745552, 75.03273214436880778, -167.1454815528550739 ) ) ;
#8863 = FACE_OUTER_BOUND ( 'NONE', #16055, .T. ) ;
#8864 = DIRECTION ( 'NONE',  ( 2.062304371594500247E-16, -1.000000000000000000, 0.000000000000000000 ) ) ;
#8865 = ORIENTED_EDGE ( 'NONE', *, *, #6394, .F. ) ;
#8866 = DIRECTION ( 'NONE',  ( 1.000000000000000000, 0.000000000000000000, 3.771137991253934490E-16 ) ) ;
#8867 = CARTESIAN_POINT ( 'NONE',  ( -67.00421887699711476, 86.78830982163884755, -15.00000000000001421 ) ) ;
#8868 = VERTEX_POINT ( 'NONE', #3497 ) ;
#8869 = PRODUCT_RELATED_PRODUCT_CATEGORY ( 'part', '', ( #17885 ) ) ;
#8870 = EDGE_LOOP ( 'NONE', ( #9950, #11463, #5055, #6786 ) ) ;
#8871 = ORIENTED_EDGE ( 'NONE', *, *, #13499, .T. ) ;
#8872 = CARTESIAN_POINT ( 'NONE',  ( -46.03642545851251100, 84.22855780814606419, -47.49999999999999289 ) ) ;
#8873 = EDGE_CURVE ( 'NONE', #10695, #6984, #6479, .T. ) ;
#8874 = DIRECTION ( 'NONE',  ( 0.000000000000000000, 0.01448153172805893840, 0.9998951371212929651 ) ) ;
#8875 =( LENGTH_UNIT ( ) NAMED_UNIT ( * ) SI_UNIT ( .MILLI., .METRE. ) );
#8876 = FACE_OUTER_BOUND ( 'NONE', #9169, .T. ) ;
#8877 = DIRECTION ( 'NONE',  ( 0.3420201433256686574, -0.9396926207859084279, 0.000000000000000000 ) ) ;
#8878 = ORIENTED_EDGE ( 'NONE', *, *, #15337, .T. ) ;
#8879 = DIRECTION ( 'NONE',  ( -1.000000000000000000, 0.000000000000000000, 0.000000000000000000 ) ) ;
#8880 = CARTESIAN_POINT ( 'NONE',  ( -68.99615306438097662, 57.94382353166266597, -15.00000000000001421 ) ) ;
#8881 = DIRECTION ( 'NONE',  ( -1.000000000000000000, -0.000000000000000000, -0.000000000000000000 ) ) ;
#8882 = DIRECTION ( 'NONE',  ( 0.000000000000000000, 0.000000000000000000, 1.000000000000000000 ) ) ;
#8883 = CARTESIAN_POINT ( 'NONE',  ( -37.02145702840577712, 90.59309441108072747, 58.52474764612693292 ) ) ;
#8884 = LINE ( 'NONE', #8970, #12575 ) ;
#8885 = ORIENTED_EDGE ( 'NONE', *, *, #5048, .F. ) ;
#8886 = CARTESIAN_POINT ( 'NONE',  ( -68.99615306438072082, 127.0588618316627105, -15.00000000000001421 ) ) ;
#8887 = DIRECTION ( 'NONE',  ( -0.000000000000000000, -0.000000000000000000, -1.000000000000000000 ) ) ;
#8888 = EDGE_LOOP ( 'NONE', ( #7822, #407, #3285, #13904 ) ) ;
#8889 = EDGE_CURVE ( 'NONE', #689, #7503, #4900, .T. ) ;
#8890 = EDGE_LOOP ( 'NONE', ( #11692, #4537, #16558, #16554 ) ) ;
#8891 = EDGE_LOOP ( 'NONE', ( #13679, #9863, #2380, #11636 ) ) ;
#8892 = CARTESIAN_POINT ( 'NONE',  ( -3.887881227897240134E-15, 5.309483803148766334, 3.803704290982293124 ) ) ;
#8893 = LINE ( 'NONE', #16163, #6346 ) ;
#8894 = CARTESIAN_POINT ( 'NONE',  ( -77.35462390582623016, 78.58944219063714343, 57.54922146810498873 ) ) ;
#8895 = DIRECTION ( 'NONE',  ( 0.9396926207859084279, 0.3420201433256686574, 0.000000000000000000 ) ) ;
#8896 = EDGE_CURVE ( 'NONE', #14192, #15440, #4986, .T. ) ;
#8897 = DIRECTION ( 'NONE',  ( 0.000000000000000000, 0.000000000000000000, 1.000000000000000000 ) ) ;
#8898 = LINE ( 'NONE', #11800, #10215 ) ;
#8899 = EDGE_LOOP ( 'NONE', ( #11476, #4923, #16594, #17102 ) ) ;
#8900 = DIRECTION ( 'NONE',  ( 1.000000000000000000, 0.000000000000000000, 0.000000000000000000 ) ) ;
#8901 = CARTESIAN_POINT ( 'NONE',  ( -57.08002265617300708, 84.22855780814606419, -15.00000000000001421 ) ) ;
#8902 = CARTESIAN_POINT ( 'NONE',  ( -58.95655619609375009, 74.15281352429524020, -167.1454815528550739 ) ) ;
#8903 = EDGE_LOOP ( 'NONE', ( #16683, #2654, #4193, #15832 ) ) ;
#8904 = CYLINDRICAL_SURFACE ( 'NONE', #4635, 7.500000000000007105 ) ;
#8905 = CARTESIAN_POINT ( 'NONE',  ( -67.59262256747317110, 57.88796029049329661, 26.35917033480641436 ) ) ;
#8906 = ORIENTED_EDGE ( 'NONE', *, *, #7187, .T. ) ;
#8907 = EDGE_CURVE ( 'NONE', #8868, #14712, #9592, .T. ) ;
#8908 = EDGE_LOOP ( 'NONE', ( #4968, #5809, #12597, #5528 ) ) ;
#8909 = CARTESIAN_POINT ( 'NONE',  ( -71.24615306438070661, 134.7758360152292312, -15.00000000000001421 ) ) ;
#8910 = DIRECTION ( 'NONE',  ( -1.000000000000000000, 1.354062621505947576E-15, 1.692578276882434470E-16 ) ) ;
#8911 = CARTESIAN_POINT ( 'NONE',  ( -107.5926225674731711, 61.64996188551983636, 25.00000000000000000 ) ) ;
#8912 = EDGE_CURVE ( 'NONE', #2797, #11561, #13793, .T. ) ;
#8913 = ORIENTED_EDGE ( 'NONE', *, *, #11144, .F. ) ;
#8914 = EDGE_CURVE ( 'NONE', #2040, #2137, #4517, .T. ) ;
#8915 = ORIENTED_EDGE ( 'NONE', *, *, #1025, .T. ) ;
#8916 = VECTOR ( 'NONE', #9203, 1000.000000000000000 ) ;
#8917 = CARTESIAN_POINT ( 'NONE',  ( 0.5805565836007609004, -3.752776749732712691, -6.500000000000033751 ) ) ;
#8918 = CARTESIAN_POINT ( 'NONE',  ( 0.000000000000000000, -5.629165124598954684, 3.250000000000013323 ) ) ;
#8919 = PLANE ( 'NONE',  #12438 ) ;
#8920 = CARTESIAN_POINT ( 'NONE',  ( -78.12361985383350316, 84.22855780814606419, 77.50000000000000000 ) ) ;
#8921 = ORIENTED_EDGE ( 'NONE', *, *, #13582, .F. ) ;
#8922 = CARTESIAN_POINT ( 'NONE',  ( 105.4583593777968105, 56.41207303426870112, 7.000000000000010658 ) ) ;
#8923 = VERTEX_POINT ( 'NONE', #13417 ) ;
#8924 = EDGE_CURVE ( 'NONE', #17074, #15837, #9906, .T. ) ;
#8925 = FACE_OUTER_BOUND ( 'NONE', #1909, .T. ) ;
#8926 = EDGE_LOOP ( 'NONE', ( #8348, #12080, #17538, #4221 ) ) ;
#8927 = ADVANCED_FACE ( 'NONE', ( #6292 ), #9403, .T. ) ;
#8928 = EDGE_CURVE ( 'NONE', #10355, #5064, #10619, .T. ) ;
#8929 = ADVANCED_FACE ( 'NONE', ( #9303 ), #5707, .F. ) ;
#8930 = VECTOR ( 'NONE', #15533, 1000.000000000000000 ) ;
#8931 = VERTEX_POINT ( 'NONE', #13612 ) ;
#8932 = CARTESIAN_POINT ( 'NONE',  ( -71.24615306438103346, 44.55851990456372391, -15.00000000000001421 ) ) ;
#8933 = CARTESIAN_POINT ( 'NONE',  ( -44.78895386838529902, 81.95267818613812949, 15.00000000000006928 ) ) ;
#8934 = EDGE_CURVE ( 'NONE', #1708, #11504, #12611, .T. ) ;
#8935 = VERTEX_POINT ( 'NONE', #5076 ) ;
#8936 = EDGE_CURVE ( 'NONE', #14282, #13644, #8179, .T. ) ;
#8937 = EDGE_CURVE ( 'NONE', #14417, #4127, #1366, .T. ) ;
#8938 = DIRECTION ( 'NONE',  ( -5.204170427930409450E-16, 0.000000000000000000, 1.000000000000000000 ) ) ;
#8939 = CARTESIAN_POINT ( 'NONE',  ( -68.99615306438089135, 80.54982793813027797, -15.00000000000001421 ) ) ;
#8940 = CARTESIAN_POINT ( 'NONE',  ( -127.5926225674731995, 110.5691553257988460, 22.35917033480641791 ) ) ;
#8941 = ORIENTED_EDGE ( 'NONE', *, *, #786, .F. ) ;
#8942 = EDGE_CURVE ( 'NONE', #6285, #4169, #8329, .T. ) ;
#8943 = CARTESIAN_POINT ( 'NONE',  ( -36.44155368744861079, 56.74635804676025685, 0.000000000000000000 ) ) ;
#8944 = AXIS2_PLACEMENT_3D ( 'NONE', #2495, #8203, #2788 ) ;
#8945 = DIRECTION ( 'NONE',  ( -5.204170427930409450E-16, 0.000000000000000000, 1.000000000000000000 ) ) ;
#8946 = CARTESIAN_POINT ( 'NONE',  ( -107.5926225674731853, 102.8748711238780373, -20.00000000000000355 ) ) ;
#8947 = VERTEX_POINT ( 'NONE', #9574 ) ;
#8948 = AXIS2_PLACEMENT_3D ( 'NONE', #15009, #2379, #15110 ) ;
#8949 = DIRECTION ( 'NONE',  ( 0.000000000000000000, 0.000000000000000000, 1.000000000000000000 ) ) ;
#8950 = CARTESIAN_POINT ( 'NONE',  ( -68.99615306438111872, 8.293196988130274505, -15.00000000000001421 ) ) ;
#8951 = ORIENTED_EDGE ( 'NONE', *, *, #12248, .F. ) ;
#8952 = EDGE_CURVE ( 'NONE', #17521, #7151, #12408, .T. ) ;
#8953 = EDGE_CURVE ( 'NONE', #833, #10654, #12905, .T. ) ;
#8954 = ORIENTED_EDGE ( 'NONE', *, *, #6432, .F. ) ;
#8955 = ORIENTED_EDGE ( 'NONE', *, *, #13737, .T. ) ;
#8956 = CIRCLE ( 'NONE', #8047, 4.599999999999992539 ) ;
#8957 = FACE_OUTER_BOUND ( 'NONE', #12271, .T. ) ;
#8958 = VECTOR ( 'NONE', #12473, 1000.000000000000000 ) ;
#8959 = DIRECTION ( 'NONE',  ( 0.000000000000000000, 0.000000000000000000, 1.000000000000000000 ) ) ;
#8960 = DIRECTION ( 'NONE',  ( 1.000000000000000000, 0.000000000000000000, 0.000000000000000000 ) ) ;
#8961 = DIRECTION ( 'NONE',  ( 1.000000000000000000, 0.000000000000000000, 0.000000000000000000 ) ) ;
#8962 = CARTESIAN_POINT ( 'NONE',  ( -68.99615306438083451, 102.5409764881302692, -15.00000000000001421 ) ) ;
#8963 = PLANE ( 'NONE',  #2204 ) ;
#8964 = ORIENTED_EDGE ( 'NONE', *, *, #10071, .T. ) ;
#8965 = CARTESIAN_POINT ( 'NONE',  ( -71.24615306438089135, 84.51035361522924916, 15.00000000000006928 ) ) ;
#8966 = FACE_OUTER_BOUND ( 'NONE', #523, .T. ) ;
#8967 = CARTESIAN_POINT ( 'NONE',  ( -66.27751174112272281, 84.22855780814606419, 92.50000000000000000 ) ) ;
#8968 = CARTESIAN_POINT ( 'NONE',  ( -68.99615306438106188, 35.95267498166268894, -167.1454815528550739 ) ) ;
#8969 = CARTESIAN_POINT ( 'NONE',  ( -36.05421503597830224, 85.21903647478332289, 55.04951438993911239 ) ) ;
#8970 = CARTESIAN_POINT ( 'NONE',  ( -68.99615306438079188, 108.8241617881302545, -15.00000000000001421 ) ) ;
#8971 = VECTOR ( 'NONE', #8059, 1000.000000000000000 ) ;
#8972 = VERTEX_POINT ( 'NONE', #16967 ) ;
#8973 = CARTESIAN_POINT ( 'NONE',  ( -64.09025127992788384, 59.14618053571278722, 35.00000000000000000 ) ) ;
#8974 = AXIS2_PLACEMENT_3D ( 'NONE', #10668, #16355, #9447 ) ;
#8975 = B_SPLINE_CURVE_WITH_KNOTS ( 'NONE', 3,
 ( #7716, #4810, #2202, #12031, #9415, #17730, #12212, #10529, #3413, #9135, #2289, #3705, #4914, #7913, #2013, #7994, #13428, #888, #6591, #10631 ),
 .UNSPECIFIED., .F., .F.,
 ( 4, 2, 2, 2, 2, 2, 2, 2, 2, 4 ),
 ( 0.000000000000000000, 0.001278592738658801062, 0.002557185477317602124, 0.003835778215976403185, 0.005114370954635204247, 0.006392963693294006176, 0.007671556431952806371, 0.008950149170611607433, 0.009589445539941000157, 0.01022874190927039288 ),
 .UNSPECIFIED. ) ;
#8976 = ORIENTED_EDGE ( 'NONE', *, *, #3658, .F. ) ;
#8977 = CIRCLE ( 'NONE', #11072, 3.999999999999989786 ) ;
#8978 = ORIENTED_EDGE ( 'NONE', *, *, #15689, .F. ) ;
#8979 = AXIS2_PLACEMENT_3D ( 'NONE', #10088, #18426, #2896 ) ;
#8980 = ORIENTED_EDGE ( 'NONE', *, *, #5612, .T. ) ;
#8981 = CARTESIAN_POINT ( 'NONE',  ( -63.80603561266293156, 73.69239390902558284, -15.00000000000001421 ) ) ;
#8982 = LINE ( 'NONE', #10114, #991 ) ;
#8983 = AXIS2_PLACEMENT_3D ( 'NONE', #4123, #14240, #4308 ) ;
#8984 = CARTESIAN_POINT ( 'NONE',  ( -76.76056308706507991, 76.77737988954069692, 63.48723832607239359 ) ) ;
#8985 = CARTESIAN_POINT ( 'NONE',  ( -71.24615306438079188, 113.6735582045637045, -167.1454815528550739 ) ) ;
#8986 = LINE ( 'NONE', #17394, #3888 ) ;
#8987 = VECTOR ( 'NONE', #17206, 1000.000000000000000 ) ;
#8988 = DIRECTION ( 'NONE',  ( 0.000000000000000000, -5.551115123125748806E-17, -1.000000000000000000 ) ) ;
#8989 = DIRECTION ( 'NONE',  ( 1.000000000000000000, 0.000000000000000000, 0.000000000000000000 ) ) ;
#8990 = AXIS2_PLACEMENT_3D ( 'NONE', #15599, #2597, #896 ) ;
#8991 = ORIENTED_EDGE ( 'NONE', *, *, #6495, .T. ) ;
#8992 = EDGE_CURVE ( 'NONE', #12749, #7713, #12588, .T. ) ;
#8993 = CARTESIAN_POINT ( 'NONE',  ( -107.5926225674731711, 57.88796029049330372, 26.35917033480641436 ) ) ;
#8994 = LINE ( 'NONE', #1878, #12959 ) ;
#8995 = LINE ( 'NONE', #4757, #16408 ) ;
#8996 = VERTEX_POINT ( 'NONE', #9963 ) ;
#8997 = EDGE_CURVE ( 'NONE', #11177, #15813, #8563, .T. ) ;
#8998 = AXIS2_PLACEMENT_3D ( 'NONE', #10228, #12693, #14272 ) ;
#8999 = PLANE ( 'NONE',  #13909 ) ;
#9000 = DIRECTION ( 'NONE',  ( -5.204170427930409450E-16, 0.000000000000000000, 1.000000000000000000 ) ) ;
#9001 = ORIENTED_EDGE ( 'NONE', *, *, #8374, .F. ) ;
#9002 = VECTOR ( 'NONE', #4804, 1000.000000000000000 ) ;
#9003 = VECTOR ( 'NONE', #10247, 1000.000000000000227 ) ;
#9004 = ORIENTED_EDGE ( 'NONE', *, *, #12014, .F. ) ;
#9005 = CYLINDRICAL_SURFACE ( 'NONE', #7038, 9.197489084949710403 ) ;
#9006 = LINE ( 'NONE', #669, #14185 ) ;
#9007 = DIRECTION ( 'NONE',  ( 0.000000000000000000, 0.000000000000000000, 1.000000000000000000 ) ) ;
#9008 = ORIENTED_EDGE ( 'NONE', *, *, #14548, .F. ) ;
#9009 = ORIENTED_EDGE ( 'NONE', *, *, #14812, .F. ) ;
#9010 = CYLINDRICAL_SURFACE ( 'NONE', #5704, 5.000000000000000000 ) ;
#9011 = CARTESIAN_POINT ( 'NONE',  ( -49.65031598894605480, 92.07579602767992810, -167.1454815528550739 ) ) ;
#9012 = SPHERICAL_SURFACE ( 'NONE', #2872, 17.12963335357822103 ) ;
#9013 = CARTESIAN_POINT ( 'NONE',  ( -75.23640716657462235, 71.26406042838958399, 102.5000000000000000 ) ) ;
#9014 = VECTOR ( 'NONE', #12282, 1000.000000000000000 ) ;
#9015 = VECTOR ( 'NONE', #2558, 1000.000000000000114 ) ;
#9016 = ORIENTED_EDGE ( 'NONE', *, *, #17728, .F. ) ;
#9017 = DIRECTION ( 'NONE',  ( 0.000000000000000000, 1.000000000000000000, 0.000000000000000000 ) ) ;
#9018 = VERTEX_POINT ( 'NONE', #12690 ) ;
#9019 = CARTESIAN_POINT ( 'NONE',  ( -71.24615306438072082, 113.6735582045637329, 15.00000000000006928 ) ) ;
#9020 = VERTEX_POINT ( 'NONE', #15670 ) ;
#9021 = CIRCLE ( 'NONE', #15292, 45.40389983439752086 ) ;
#9022 = EDGE_CURVE ( 'NONE', #1535, #17780, #4075, .T. ) ;
#9023 = ORIENTED_EDGE ( 'NONE', *, *, #3446, .T. ) ;
#9024 = ORIENTED_EDGE ( 'NONE', *, *, #8702, .F. ) ;
#9025 = VECTOR ( 'NONE', #9635, 1000.000000000000000 ) ;
#9026 =( NAMED_UNIT ( * ) SI_UNIT ( $, .STERADIAN. ) SOLID_ANGLE_UNIT ( ) );
#9027 = DIRECTION ( 'NONE',  ( 0.9396926207859069846, 0.3420201433256723766, 0.000000000000000000 ) ) ;
#9028 = VERTEX_POINT ( 'NONE', #14269 ) ;
#9029 = CARTESIAN_POINT ( 'NONE',  ( -81.37409655828226107, -91.08423613455721579, -38.97384619189710975 ) ) ;
#9030 = CYLINDRICAL_SURFACE ( 'NONE', #14099, 4.599999999999992539 ) ;
#9031 = EDGE_CURVE ( 'NONE', #7261, #7647, #3602, .T. ) ;
#9032 = LINE ( 'NONE', #10427, #10293 ) ;
#9033 = ORIENTED_EDGE ( 'NONE', *, *, #16836, .T. ) ;
#9034 = EDGE_CURVE ( 'NONE', #4979, #7322, #8840, .T. ) ;
#9035 = VECTOR ( 'NONE', #12583, 1000.000000000000000 ) ;
#9036 = FACE_OUTER_BOUND ( 'NONE', #16364, .T. ) ;
#9037 = CARTESIAN_POINT ( 'NONE',  ( -68.99615306438067819, 146.5232735881302801, -167.1454815528550739 ) ) ;
#9038 = LINE ( 'NONE', #7533, #13511 ) ;
#9039 = ORIENTED_EDGE ( 'NONE', *, *, #13367, .F. ) ;
#9040 = VECTOR ( 'NONE', #6561, 1000.000000000000000 ) ;
#9041 = DIRECTION ( 'NONE',  ( -1.000000000000000000, -0.000000000000000000, -0.000000000000000000 ) ) ;
#9042 = EDGE_CURVE ( 'NONE', #14175, #7136, #16471, .T. ) ;
#9043 = EDGE_CURVE ( 'NONE', #7186, #13900, #6174, .T. ) ;
#9044 = PLANE ( 'NONE',  #15826 ) ;
#9045 = EDGE_CURVE ( 'NONE', #18127, #14885, #494, .T. ) ;
#9046 = ORIENTED_EDGE ( 'NONE', *, *, #1173, .F. ) ;
#9047 = ORIENTED_EDGE ( 'NONE', *, *, #16664, .T. ) ;
#9048 = AXIS2_PLACEMENT_3D ( 'NONE', #8341, #14053, #5782 ) ;
#9049 = ORIENTED_EDGE ( 'NONE', *, *, #17169, .T. ) ;
#9050 = FACE_OUTER_BOUND ( 'NONE', #13955, .T. ) ;
#9051 = ADVANCED_FACE ( 'NONE', ( #7689 ), #5058, .F. ) ;
#9052 = AXIS2_PLACEMENT_3D ( 'NONE', #10379, #3182, #11794 ) ;
#9053 = CIRCLE ( 'NONE', #2483, 4.599999999999992539 ) ;
#9054 = DIRECTION ( 'NONE',  ( 0.000000000000000000, 0.000000000000000000, 1.000000000000000000 ) ) ;
#9055 = LINE ( 'NONE', #16053, #12663 ) ;
#9056 = DIRECTION ( 'NONE',  ( 0.000000000000000000, 0.000000000000000000, 1.000000000000000000 ) ) ;
#9057 = ORIENTED_EDGE ( 'NONE', *, *, #17130, .T. ) ;
#9058 = FACE_OUTER_BOUND ( 'NONE', #1133, .T. ) ;
#9059 = DIRECTION ( 'NONE',  ( 0.000000000000000000, 1.000000000000000000, 0.000000000000000000 ) ) ;
#9060 = ADVANCED_FACE ( 'NONE', ( #13397 ), #10775, .T. ) ;
#9061 = LINE ( 'NONE', #1947, #173 ) ;
#9062 = FACE_OUTER_BOUND ( 'NONE', #3195, .T. ) ;
#9063 = EDGE_CURVE ( 'NONE', #10340, #12345, #17233, .T. ) ;
#9064 = CARTESIAN_POINT ( 'NONE',  ( -36.03642545851253232, 84.72841810161554577, 55.00000000000002842 ) ) ;
#9065 = VERTEX_POINT ( 'NONE', #3379 ) ;
#9066 = AXIS2_PLACEMENT_3D ( 'NONE', #7170, #11211, #15497 ) ;
#9067 = DIRECTION ( 'NONE',  ( 0.000000000000000000, 0.000000000000000000, 1.000000000000000000 ) ) ;
#9068 = ORIENTED_EDGE ( 'NONE', *, *, #16236, .T. ) ;
#9069 = EDGE_CURVE ( 'NONE', #10128, #5779, #17963, .T. ) ;
#9070 = CARTESIAN_POINT ( 'NONE',  ( -68.99615306438106188, 35.95267498166268894, 15.00000000000006928 ) ) ;
#9071 = CIRCLE ( 'NONE', #2195, 21.04359719766049608 ) ;
#9072 = VERTEX_POINT ( 'NONE', #15073 ) ;
#9073 = AXIS2_PLACEMENT_3D ( 'NONE', #13654, #746, #17658 ) ;
#9074 = ORIENTED_EDGE ( 'NONE', *, *, #792, .F. ) ;
#9075 = AXIS2_PLACEMENT_3D ( 'NONE', #6456, #3557, #16463 ) ;
#9076 = EDGE_LOOP ( 'NONE', ( #16411, #10232, #18286, #15065 ) ) ;
#9077 = CARTESIAN_POINT ( 'NONE',  ( -56.41614838398844256, 95.01461175692088545, 15.00000000000006928 ) ) ;
#9078 = DIRECTION ( 'NONE',  ( 0.000000000000000000, 1.000000000000000000, 0.000000000000000000 ) ) ;
#9079 = CARTESIAN_POINT ( 'NONE',  ( -68.99615306438094819, 52.27549408813023746, -167.1454815528550739 ) ) ;
#9080 = DIRECTION ( 'NONE',  ( 0.000000000000000000, 1.000000000000000000, 0.000000000000000000 ) ) ;
#9081 = CARTESIAN_POINT ( 'NONE',  ( 103.5381772159376084, -151.5628872026272802, -36.00000000000000000 ) ) ;
#9082 = FACE_OUTER_BOUND ( 'NONE', #5429, .T. ) ;
#9083 = AXIS2_PLACEMENT_3D ( 'NONE', #12582, #2467, #11075 ) ;
#9084 = CARTESIAN_POINT ( 'NONE',  ( -49.75809927370887920, 76.28065702765852052, -167.1454815528550739 ) ) ;
#9085 = ORIENTED_EDGE ( 'NONE', *, *, #10743, .F. ) ;
#9086 = CARTESIAN_POINT ( 'NONE',  ( -42.13578017738746695, 48.33287759230859137, -28.43492242011098625 ) ) ;
#9087 = LINE ( 'NONE', #480, #4859 ) ;
#9088 = FACE_OUTER_BOUND ( 'NONE', #1492, .T. ) ;
#9089 = ORIENTED_EDGE ( 'NONE', *, *, #4376, .T. ) ;
#9090 = VECTOR ( 'NONE', #15853, 1000.000000000000000 ) ;
#9091 = DIRECTION ( 'NONE',  ( 1.156482317317869999E-16, 0.000000000000000000, 1.000000000000000000 ) ) ;
#9092 = DIRECTION ( 'NONE',  ( 0.000000000000000000, 1.000000000000000000, 0.000000000000000000 ) ) ;
#9093 = ORIENTED_EDGE ( 'NONE', *, *, #13392, .T. ) ;
#9094 = VECTOR ( 'NONE', #10298, 1000.000000000000114 ) ;
#9095 = AXIS2_PLACEMENT_3D ( 'NONE', #10076, #14372, #16903 ) ;
#9096 = CIRCLE ( 'NONE', #8186, 5.654315315325682434 ) ;
#9097 = EDGE_LOOP ( 'NONE', ( #13734, #9672, #7143, #18336 ) ) ;
#9098 = DIRECTION ( 'NONE',  ( -1.000000000000000000, -0.000000000000000000, -0.000000000000000000 ) ) ;
#9099 = DIRECTION ( 'NONE',  ( -1.000000000000000000, -0.000000000000000000, -0.000000000000000000 ) ) ;
#9100 = FACE_OUTER_BOUND ( 'NONE', #10237, .T. ) ;
#9101=STYLED_ITEM('',(#18573),#314);
#9102 = VERTEX_POINT ( 'NONE', #5158 ) ;
#9103 = CARTESIAN_POINT ( 'NONE',  ( 0.05533025579362768620, 6.264553569211829043, -2.149474931388220433 ) ) ;
#9104 = ORIENTED_EDGE ( 'NONE', *, *, #3658, .T. ) ;
#9105 = CIRCLE ( 'NONE', #154, 4.599999999999992539 ) ;
#9106 = CYLINDRICAL_SURFACE ( 'NONE', #1536, 3.999999999999989786 ) ;
#9107 = PLANE ( 'NONE',  #17368 ) ;
#9108 = LINE ( 'NONE', #2265, #1890 ) ;
#9109 = CARTESIAN_POINT ( 'NONE',  ( -111.3698580185283760, -91.24992890033504978, 9.348340137069554245 ) ) ;
#9110 = AXIS2_PLACEMENT_3D ( 'NONE', #7434, #510, #15861 ) ;
#9111 = ORIENTED_EDGE ( 'NONE', *, *, #4936, .T. ) ;
#9112 = VECTOR ( 'NONE', #1339, 1000.000000000000000 ) ;
#9113 = CYLINDRICAL_SURFACE ( 'NONE', #9245, 11.04359719766049430 ) ;
#9114 = ORIENTED_EDGE ( 'NONE', *, *, #1920, .F. ) ;
#9115 = DIRECTION ( 'NONE',  ( 0.9396926207859084279, 0.3420201433256686574, 4.890320548438448905E-16 ) ) ;
#9116 = ORIENTED_EDGE ( 'NONE', *, *, #15181, .T. ) ;
#9117 = ORIENTED_EDGE ( 'NONE', *, *, #3534, .T. ) ;
#9118 = ORIENTED_EDGE ( 'NONE', *, *, #2418, .F. ) ;
#9119 = CIRCLE ( 'NONE', #5542, 10.24900000000000055 ) ;
#9120 = VECTOR ( 'NONE', #9054, 1000.000000000000000 ) ;
#9121 = DIRECTION ( 'NONE',  ( 0.000000000000000000, 1.000000000000000000, 0.000000000000000000 ) ) ;
#9122 = ORIENTED_EDGE ( 'NONE', *, *, #577, .F. ) ;
#9123 = DIRECTION ( 'NONE',  ( 1.110223024625157172E-14, -6.938893903907068633E-16, -1.000000000000000000 ) ) ;
#9124 = DIRECTION ( 'NONE',  ( -1.000000000000000000, 0.000000000000000000, 0.000000000000000000 ) ) ;
#9125 = ORIENTED_EDGE ( 'NONE', *, *, #14808, .T. ) ;
#9126 = EDGE_CURVE ( 'NONE', #12063, #17707, #9194, .T. ) ;
#9127 = DIRECTION ( 'NONE',  ( 1.000000000000000000, 0.000000000000000000, 4.163336342344339393E-15 ) ) ;
#9128 = VERTEX_POINT ( 'NONE', #7965 ) ;
#9129 = CARTESIAN_POINT ( 'NONE',  ( 124.5381772159375942, -111.0842361345572158, 36.00000000000001421 ) ) ;
#9130 = DIRECTION ( 'NONE',  ( 7.442644330182800165E-16, -1.000000000000000000, 0.000000000000000000 ) ) ;
#9131 = ORIENTED_EDGE ( 'NONE', *, *, #5268, .F. ) ;
#9132 = VECTOR ( 'NONE', #188, 1000.000000000000000 ) ;
#9133 = AXIS2_PLACEMENT_3D ( 'NONE', #9331, #16702, #6804 ) ;
#9134 = DIRECTION ( 'NONE',  ( 0.000000000000000000, 0.000000000000000000, 1.000000000000000000 ) ) ;
#9135 = CARTESIAN_POINT ( 'NONE',  ( -78.51801170372698380, -91.96846159163195011, -42.55230335834804833 ) ) ;
#9136 = VERTEX_POINT ( 'NONE', #10872 ) ;
#9137 = ADVANCED_FACE ( 'NONE', ( #13493 ), #16565, .T. ) ;
#9138 = EDGE_CURVE ( 'NONE', #17987, #593, #16375, .T. ) ;
#9139 = ORIENTED_EDGE ( 'NONE', *, *, #16942, .F. ) ;
#9140 = CARTESIAN_POINT ( 'NONE',  ( -63.16290507965269541, 75.97988867778799715, 15.00000000000006928 ) ) ;
#9141 = DIRECTION ( 'NONE',  ( 1.119176436114069332E-16, -1.000000000000000000, -0.000000000000000000 ) ) ;
#9142 = ORIENTED_EDGE ( 'NONE', *, *, #15442, .T. ) ;
#9143 = PRODUCT_CONTEXT ( 'NONE', #7760, 'mechanical' ) ;
#9144 = CARTESIAN_POINT ( 'NONE',  ( -64.40194603863702127, 76.28065702765842104, -167.1454815528550739 ) ) ;
#9145 = DIRECTION ( 'NONE',  ( -1.000000000000000000, 0.000000000000000000, 0.000000000000000000 ) ) ;
#9146 = FACE_OUTER_BOUND ( 'NONE', #3870, .T. ) ;
#9147 = ORIENTED_EDGE ( 'NONE', *, *, #3525, .T. ) ;
#9148 = EDGE_CURVE ( 'NONE', #3167, #5425, #17661, .T. ) ;
#9149 = EDGE_CURVE ( 'NONE', #12345, #7124, #18142, .T. ) ;
#9150 = DIRECTION ( 'NONE',  ( 0.000000000000000000, 0.000000000000000000, 1.000000000000000000 ) ) ;
#9151 = PLANE ( 'NONE',  #10327 ) ;
#9152 = DIRECTION ( 'NONE',  ( -1.000000000000000000, 2.693970411862685384E-15, 0.000000000000000000 ) ) ;
#9153 = DIRECTION ( 'NONE',  ( 0.000000000000000000, 0.000000000000000000, 1.000000000000000000 ) ) ;
#9154 = LINE ( 'NONE', #5212, #17095 ) ;
#9155 = ORIENTED_EDGE ( 'NONE', *, *, #10409, .F. ) ;
#9156 = ADVANCED_FACE ( 'NONE', ( #16952, #3943 ), #18368, .T. ) ;
#9157 = CARTESIAN_POINT ( 'NONE',  ( -71.24615306438070661, 138.8062994045637311, -15.00000000000001421 ) ) ;
#9158 = CARTESIAN_POINT ( 'NONE',  ( -68.99615306438111872, 10.81993378166265529, 15.00000000000006928 ) ) ;
#9159 = EDGE_LOOP ( 'NONE', ( #12908, #17004, #1488, #16898 ) ) ;
#9160 = DIRECTION ( 'NONE',  ( -0.9396926207859158664, 0.3420201433256481738, 0.000000000000000000 ) ) ;
#9161 = EDGE_CURVE ( 'NONE', #4200, #274, #3042, .T. ) ;
#9162 = DIRECTION ( 'NONE',  ( 0.000000000000000000, 0.000000000000000000, 1.000000000000000000 ) ) ;
#9163 = VERTEX_POINT ( 'NONE', #4228 ) ;
#9164 = EDGE_CURVE ( 'NONE', #7136, #4354, #6011, .T. ) ;
#9165 = VERTEX_POINT ( 'NONE', #12475 ) ;
#9166 = ADVANCED_FACE ( 'NONE', ( #11060 ), #15365, .T. ) ;
#9167 = EDGE_CURVE ( 'NONE', #12615, #10671, #18077, .T. ) ;
#9168 = FACE_OUTER_BOUND ( 'NONE', #1295, .T. ) ;
#9169 = EDGE_LOOP ( 'NONE', ( #5751, #4172, #4744, #7067 ) ) ;
#9170 = LINE ( 'NONE', #14856, #15064 ) ;
#9171 = DIRECTION ( 'NONE',  ( -1.000000000000000000, 0.000000000000000000, 0.000000000000000000 ) ) ;
#9172 = CARTESIAN_POINT ( 'NONE',  ( -107.5926225674732137, 107.8748711238780373, -35.00000000000000000 ) ) ;
#9173 = ADVANCED_FACE ( 'NONE', ( #16747 ), #11264, .T. ) ;
#9174 = EDGE_CURVE ( 'NONE', #6461, #1535, #6758, .T. ) ;
#9175 = CARTESIAN_POINT ( 'NONE',  ( 4.699999999999995737, 7.505553499465141165, -1.387778780781445676E-14 ) ) ;
#9176 = DIRECTION ( 'NONE',  ( 0.9396926207859110924, 0.3420201433256612189, -1.086737899652992973E-16 ) ) ;
#9177 = DIRECTION ( 'NONE',  ( -1.000000000000000000, 6.400974180244839938E-15, 0.000000000000000000 ) ) ;
#9178 = ORIENTED_EDGE ( 'NONE', *, *, #6283, .F. ) ;
#9179 = CARTESIAN_POINT ( 'NONE',  ( -68.99615306438106188, 26.52789703166272162, -167.1454815528550739 ) ) ;
#9180 = LINE ( 'NONE', #7954, #9358 ) ;
#9181 = FACE_OUTER_BOUND ( 'NONE', #3015, .T. ) ;
#9182 = ORIENTED_EDGE ( 'NONE', *, *, #11444, .F. ) ;
#9183 = DIRECTION ( 'NONE',  ( 0.000000000000000000, 1.000000000000000000, -0.000000000000000000 ) ) ;
#9184 = DIRECTION ( 'NONE',  ( 1.156482317317869999E-16, 0.000000000000000000, 1.000000000000000000 ) ) ;
#9185 = ORIENTED_EDGE ( 'NONE', *, *, #16366, .T. ) ;
#9186 = EDGE_CURVE ( 'NONE', #9018, #11293, #12564, .T. ) ;
#9187 = EDGE_LOOP ( 'NONE', ( #2134, #16031, #8381, #10981 ) ) ;
#9188 = DIRECTION ( 'NONE',  ( 0.000000000000000000, 0.000000000000000000, 1.000000000000000000 ) ) ;
#9189 = CARTESIAN_POINT ( 'NONE',  ( -66.27474722583565381, 78.55081803573735044, -15.00000000000001421 ) ) ;
#9190 = CARTESIAN_POINT ( 'NONE',  ( 5.233202738124664855, -46.83756720124470263, 57.00000000000000000 ) ) ;
#9191 = DIRECTION ( 'NONE',  ( 0.3420201433256724322, -0.9396926207859070956, 0.000000000000000000 ) ) ;
#9192 = VERTEX_POINT ( 'NONE', #2734 ) ;
#9193 = PLANE ( 'NONE',  #1018 ) ;
#9194 = LINE ( 'NONE', #14884, #8110 ) ;
#9195 = ORIENTED_EDGE ( 'NONE', *, *, #11899, .F. ) ;
#9196 = CARTESIAN_POINT ( 'NONE',  ( -70.06856178257680767, 110.5691553257988460, -22.35917033480641791 ) ) ;
#9197 = CARTESIAN_POINT ( 'NONE',  ( -71.24615306438120399, -0.3126479347707321610, -15.00000000000001421 ) ) ;
#9198 = CARTESIAN_POINT ( 'NONE',  ( -68.99615306438120399, -1.131580961869733448, -167.1454815528550739 ) ) ;
#9199 = CARTESIAN_POINT ( 'NONE',  ( -71.24615306438120399, -0.3126479347707321610, 15.00000000000006928 ) ) ;
#9200 = ORIENTED_EDGE ( 'NONE', *, *, #2518, .F. ) ;
#9201 = DIRECTION ( 'NONE',  ( 0.000000000000000000, 0.000000000000000000, -1.000000000000000000 ) ) ;
#9202 = ORIENTED_EDGE ( 'NONE', *, *, #8924, .F. ) ;
#9203 = DIRECTION ( 'NONE',  ( 0.000000000000000000, 0.000000000000000000, 1.000000000000000000 ) ) ;
#9204 = VERTEX_POINT ( 'NONE', #15260 ) ;
#9205 = ORIENTED_EDGE ( 'NONE', *, *, #2166, .T. ) ;
#9206 = FILL_AREA_STYLE ('',( #12296 ) ) ;
#9207 = VECTOR ( 'NONE', #9295, 1000.000000000000000 ) ;
#9208 = DIRECTION ( 'NONE',  ( 0.000000000000000000, 0.000000000000000000, 1.000000000000000000 ) ) ;
#9209 = ORIENTED_EDGE ( 'NONE', *, *, #3882, .F. ) ;
#9210 = CARTESIAN_POINT ( 'NONE',  ( -68.99615306438080609, 105.0677132816627051, -15.00000000000001421 ) ) ;
#9211 = LINE ( 'NONE', #3692, #2527 ) ;
#9212 = ORIENTED_EDGE ( 'NONE', *, *, #17178, .T. ) ;
#9213 = DIRECTION ( 'NONE',  ( 0.000000000000000000, 0.000000000000000000, 1.000000000000000000 ) ) ;
#9214 = EDGE_LOOP ( 'NONE', ( #2386, #3508, #2345, #17801 ) ) ;
#9215 = FACE_OUTER_BOUND ( 'NONE', #9214, .T. ) ;
#9216 = LINE ( 'NONE', #2009, #16502 ) ;
#9218 = ORIENTED_EDGE ( 'NONE', *, *, #11258, .T. ) ;
#9217 = EDGE_CURVE ( 'NONE', #18436, #2297, #4137, .T. ) ;
#9219 = PLANE ( 'NONE',  #13010 ) ;
#9220 = CIRCLE ( 'NONE', #11335, 10.24900000000000055 ) ;
#9221 = DIRECTION ( 'NONE',  ( 0.000000000000000000, 0.000000000000000000, -1.000000000000000000 ) ) ;
#9222 = VERTEX_POINT ( 'NONE', #2449 ) ;
#9223 = VERTEX_POINT ( 'NONE', #13772 ) ;
#9224 = DIRECTION ( 'NONE',  ( 1.156482317317869999E-16, 0.000000000000000000, 1.000000000000000000 ) ) ;
#9225 = DIRECTION ( 'NONE',  ( 1.000000000000000000, 0.000000000000000000, 3.771137991253923150E-16 ) ) ;
#9226 = ORIENTED_EDGE ( 'NONE', *, *, #13607, .F. ) ;
#9227 = DIRECTION ( 'NONE',  ( 0.000000000000000000, 1.000000000000000000, 0.000000000000000000 ) ) ;
#9228 = CARTESIAN_POINT ( 'NONE',  ( 5.233202738124664855, -19.34983604512936495, 54.79921157549230770 ) ) ;
#9229 = AXIS2_PLACEMENT_3D ( 'NONE', #11744, #11646, #4626 ) ;
#9230 = CARTESIAN_POINT ( 'NONE',  ( -57.08002265617300708, 84.22855780814606419, -7.000000000000013323 ) ) ;
#9231 = ORIENTED_EDGE ( 'NONE', *, *, #11802, .T. ) ;
#9232 = LINE ( 'NONE', #14747, #4504 ) ;
#9233 = CARTESIAN_POINT ( 'NONE',  ( -71.24615306438087714, 85.39922435456371375, -15.00000000000001421 ) ) ;
#9234 = CARTESIAN_POINT ( 'NONE',  ( -57.08002265617300708, 84.22855780814606419, -167.1454815528550739 ) ) ;
#9235 = LINE ( 'NONE', #16249, #14126 ) ;
#9236 = ORIENTED_EDGE ( 'NONE', *, *, #15769, .F. ) ;
#9237 = EDGE_CURVE ( 'NONE', #715, #7744, #6661, .T. ) ;
#9238 = CARTESIAN_POINT ( 'NONE',  ( -68.99615306438094819, 51.66063823166267355, -15.00000000000001421 ) ) ;
#9239 = CARTESIAN_POINT ( 'NONE',  ( -65.06546592763146464, -96.08423613455721579, 45.05044770573184110 ) ) ;
#9240 = ORIENTED_EDGE ( 'NONE', *, *, #10870, .T. ) ;
#9241 = DIRECTION ( 'NONE',  ( -0.7071067811864494290, 0.000000000000000000, 0.7071067811866454944 ) ) ;
#9242 = CARTESIAN_POINT ( 'NONE',  ( -71.24615306438114715, 12.25372266522925457, 15.00000000000006928 ) ) ;
#9243 = VERTEX_POINT ( 'NONE', #1241 ) ;
#9244 = EDGE_CURVE ( 'NONE', #827, #16099, #1549, .T. ) ;
#9245 = AXIS2_PLACEMENT_3D ( 'NONE', #14804, #9292, #1994 ) ;
#9246 = ORIENTED_EDGE ( 'NONE', *, *, #4678, .T. ) ;
#9247 = EDGE_CURVE ( 'NONE', #7512, #1261, #16854, .T. ) ;
#9248 = VECTOR ( 'NONE', #7874, 1000.000000000000000 ) ;
#9249 = CARTESIAN_POINT ( 'NONE',  ( -107.5926225674731711, 57.88796029049330372, -22.33417033480641223 ) ) ;
#9250 = VERTEX_POINT ( 'NONE', #6843 ) ;
#9251 = DIRECTION ( 'NONE',  ( 1.000000000000000000, 0.000000000000000000, 0.000000000000000000 ) ) ;
#9252 = DIRECTION ( 'NONE',  ( 0.000000000000000000, 0.000000000000000000, 1.000000000000000000 ) ) ;
#9253 = PLANE ( 'NONE',  #15721 ) ;
#9254 = DIRECTION ( 'NONE',  ( 0.000000000000000000, 0.000000000000000000, -1.000000000000000000 ) ) ;
#9255 = EDGE_CURVE ( 'NONE', #8042, #5082, #8436, .T. ) ;
#9256 = CARTESIAN_POINT ( 'NONE',  ( -70.85175816390371040, -141.5628872026273086, -57.00000000000000000 ) ) ;
#9257 = CARTESIAN_POINT ( 'NONE',  ( -194.4437806548868934, -151.5628872026273086, -18.23991632971910803 ) ) ;
#9258 = EDGE_LOOP ( 'NONE', ( #7305, #18042, #12374, #8060 ) ) ;
#9260 = EDGE_CURVE ( 'NONE', #9888, #3544, #11164, .T. ) ;
#9259 = AXIS2_PLACEMENT_3D ( 'NONE', #21, #10122, #15827 ) ;
#9261 = ADVANCED_FACE ( 'NONE', ( #8343 ), #7485, .F. ) ;
#9262 = CARTESIAN_POINT ( 'NONE',  ( -74.87388236440091305, 60.86317103097213277, -23.67979665430766190 ) ) ;
#9263 = AXIS2_PLACEMENT_3D ( 'NONE', #14591, #1773, #6069 ) ;
#9264 = LINE ( 'NONE', #7400, #6875 ) ;
#9265 = EDGE_LOOP ( 'NONE', ( #14340, #5702, #1335, #13912 ) ) ;
#9266 = CARTESIAN_POINT ( 'NONE',  ( -57.08002265617300708, 84.22855780814606419, -15.00000000000001421 ) ) ;
#9267 = ORIENTED_EDGE ( 'NONE', *, *, #8896, .F. ) ;
#9268 = EDGE_CURVE ( 'NONE', #14872, #293, #14513, .T. ) ;
#9269 = ADVANCED_FACE ( 'NONE', ( #6072 ), #12942, .T. ) ;
#9270 = EDGE_CURVE ( 'NONE', #103, #11183, #5891, .T. ) ;
#9271 = VECTOR ( 'NONE', #13018, 1000.000000000000000 ) ;
#9272 = ORIENTED_EDGE ( 'NONE', *, *, #10900, .T. ) ;
#9273 = EDGE_CURVE ( 'NONE', #15127, #4073, #1691, .T. ) ;
#9274 = VECTOR ( 'NONE', #13720, 1000.000000000000000 ) ;
#9275 = AXIS2_PLACEMENT_3D ( 'NONE', #2408, #8114, #17930 ) ;
#9276 = DIRECTION ( 'NONE',  ( 0.000000000000000000, 0.000000000000000000, 1.000000000000000000 ) ) ;
#9277 = DIRECTION ( 'NONE',  ( 0.000000000000000000, 0.000000000000000000, 1.000000000000000000 ) ) ;
#9278 = DIRECTION ( 'NONE',  ( 0.000000000000000000, 0.000000000000000000, 1.000000000000000000 ) ) ;
#9279 = DIRECTION ( 'NONE',  ( 1.000000000000000000, -0.000000000000000000, -0.000000000000000000 ) ) ;
#9280 = EDGE_CURVE ( 'NONE', #11545, #4878, #3186, .T. ) ;
#9281 = VERTEX_POINT ( 'NONE', #10301 ) ;
#9282 = CARTESIAN_POINT ( 'NONE',  ( -58.95655619609375009, 74.15281352429524020, -15.00000000000001421 ) ) ;
#9283 = CARTESIAN_POINT ( 'NONE',  ( 0.000000000000000000, 5.629165124598635828, -3.250000000000016875 ) ) ;
#9284 = VERTEX_POINT ( 'NONE', #9940 ) ;
#9285 = CARTESIAN_POINT ( 'NONE',  ( -57.08002265617300708, 84.22855780814606419, 35.00000000000000000 ) ) ;
#9286 = CYLINDRICAL_SURFACE ( 'NONE', #11712, 12.50000000000001066 ) ;
#9287 = CARTESIAN_POINT ( 'NONE',  ( -77.09746718839080870, 90.72084218871722783, 58.73700743486453746 ) ) ;
#9288 = DIRECTION ( 'NONE',  ( 1.000000000000000000, 2.062304371594500494E-16, 0.000000000000000000 ) ) ;
#9289 = ORIENTED_EDGE ( 'NONE', *, *, #16336, .T. ) ;
#9290 = ADVANCED_FACE ( 'NONE', ( #10035 ), #5808, .T. ) ;
#9291 = EDGE_CURVE ( 'NONE', #1462, #16981, #8898, .T. ) ;
#9292 = DIRECTION ( 'NONE',  ( 0.000000000000000000, 0.000000000000000000, -1.000000000000000000 ) ) ;
#9293 = EDGE_LOOP ( 'NONE', ( #17949, #1334 ) ) ;
#9294 = AXIS2_PLACEMENT_3D ( 'NONE', #10645, #15123, #7730 ) ;
#9295 = DIRECTION ( 'NONE',  ( 0.000000000000000000, 0.000000000000000000, 1.000000000000000000 ) ) ;
#9296 = ORIENTED_EDGE ( 'NONE', *, *, #4350, .T. ) ;
#9297 = ORIENTED_EDGE ( 'NONE', *, *, #14267, .T. ) ;
#9298 = VECTOR ( 'NONE', #2762, 1000.000000000000000 ) ;
#9299 = DIRECTION ( 'NONE',  ( 0.000000000000000000, 0.000000000000000000, -1.000000000000000000 ) ) ;
#9300 = ORIENTED_EDGE ( 'NONE', *, *, #9, .T. ) ;
#9301 = VECTOR ( 'NONE', #3206, 1000.000000000000000 ) ;
#9302 = CIRCLE ( 'NONE', #7804, 10.65431531532568243 ) ;
#9303 = FACE_OUTER_BOUND ( 'NONE', #2062, .T. ) ;
#9304 = CARTESIAN_POINT ( 'NONE',  ( 0.000000000000000000, 0.000000000000000000, 0.000000000000000000 ) ) ;
#9305 = ORIENTED_EDGE ( 'NONE', *, *, #4271, .F. ) ;
#9306 = CARTESIAN_POINT ( 'NONE',  ( -71.24615306438103346, 46.81124181522922356, 15.00000000000006928 ) ) ;
#9307 = VERTEX_POINT ( 'NONE', #2836 ) ;
#9308 = CARTESIAN_POINT ( 'NONE',  ( -47.76080550507955280, 75.89776002577458769, 15.00000000000006928 ) ) ;
#9309 = CARTESIAN_POINT ( 'NONE',  ( 0.000000000000000000, -91.08423613455721579, 5.654315315325685987 ) ) ;
#9310 = ORIENTED_EDGE ( 'NONE', *, *, #18311, .T. ) ;
#9311 = CONICAL_SURFACE ( 'NONE', #5120, 6.500000000000039968, 1.047197551196600296 ) ;
#9312 = CARTESIAN_POINT ( 'NONE',  ( -68.99615306438083451, 101.9261206316626698, 15.00000000000006928 ) ) ;
#9313 = DIRECTION ( 'NONE',  ( -1.000000000000000000, 0.000000000000000000, 0.000000000000000000 ) ) ;
#9314 = CIRCLE ( 'NONE', #15882, 3.999999999999989786 ) ;
#9315 = CIRCLE ( 'NONE', #15610, 2.168074330098864078 ) ;
#9316 = VERTEX_POINT ( 'NONE', #17222 ) ;
#9317 = ORIENTED_EDGE ( 'NONE', *, *, #9609, .T. ) ;
#9318 = VERTEX_POINT ( 'NONE', #13202 ) ;
#9320 = EDGE_CURVE ( 'NONE', #17849, #3192, #14593, .T. ) ;
#9319 = CYLINDRICAL_SURFACE ( 'NONE', #3390, 12.49999999999999112 ) ;
#9321 = DIRECTION ( 'NONE',  ( 0.3420201433256407353, -0.9396926207859186420, 0.000000000000000000 ) ) ;
#9322 = CIRCLE ( 'NONE', #13216, 12.49999999999999112 ) ;
#9323 = CARTESIAN_POINT ( 'NONE',  ( -94.45685920050698314, -47.21335801510345220, 15.00000000000006928 ) ) ;
#9324 = CARTESIAN_POINT ( 'NONE',  ( -76.91951136665340982, 77.21161119120515082, 65.15931570389709293 ) ) ;
#9325 = CARTESIAN_POINT ( 'NONE',  ( -70.85175816390371040, -141.5628872026273086, 57.00000000000000000 ) ) ;
#9326 = LINE ( 'NONE', #12521, #6376 ) ;
#9327 = VERTEX_POINT ( 'NONE', #205 ) ;
#9328 = EDGE_CURVE ( 'NONE', #16319, #9465, #1775, .T. ) ;
#9329 = CARTESIAN_POINT ( 'NONE',  ( -92.59262256747321373, 117.8748711238780373, -35.00000000000000000 ) ) ;
#9330 = VECTOR ( 'NONE', #10350, 1000.000000000000114 ) ;
#9331 = CARTESIAN_POINT ( 'NONE',  ( -70.71978124295668522, -96.08423613455721579, -28.18308811886538479 ) ) ;
#9332 = PRESENTATION_STYLE_ASSIGNMENT (( #3810 ) ) ;
#9333 = DIRECTION ( 'NONE',  ( -0.000000000000000000, -0.000000000000000000, -1.000000000000000000 ) ) ;
#9334 = ORIENTED_EDGE ( 'NONE', *, *, #6673, .T. ) ;
#9335 = CARTESIAN_POINT ( 'NONE',  ( -57.35243698450333483, 71.73152654333280509, -167.1454815528550739 ) ) ;
#9336 = CYLINDRICAL_SURFACE ( 'NONE', #17329, 5.654315315325682434 ) ;
#9337 = ORIENTED_EDGE ( 'NONE', *, *, #4046, .T. ) ;
#9338 = AXIS2_PLACEMENT_3D ( 'NONE', #4894, #3495, #9299 ) ;
#9339 = LINE ( 'NONE', #9521, #8396 ) ;
#9340 = DIRECTION ( 'NONE',  ( -1.000000000000000000, 0.000000000000000000, 1.387778780781446662E-16 ) ) ;
#9341 = ORIENTED_EDGE ( 'NONE', *, *, #11337, .T. ) ;
#9342 = ORIENTED_EDGE ( 'NONE', *, *, #4548, .T. ) ;
#9343 = CIRCLE ( 'NONE', #12331, 9.999999999999994671 ) ;
#9344 = VECTOR ( 'NONE', #15937, 1000.000000000000000 ) ;
#9345 = CARTESIAN_POINT ( 'NONE',  ( -102.5926225674731853, 102.8748711238780373, 20.00000000000000355 ) ) ;
#9346 = ORIENTED_EDGE ( 'NONE', *, *, #8477, .T. ) ;
#9347 = DIRECTION ( 'NONE',  ( -1.000000000000000000, -0.000000000000000000, -0.000000000000000000 ) ) ;
#9348 = DIRECTION ( 'NONE',  ( 1.000000000000000000, 2.062304371594500494E-16, 0.000000000000000000 ) ) ;
#9349 = CARTESIAN_POINT ( 'NONE',  ( -67.59262256747317110, 61.53592931583062153, -28.00000000000000355 ) ) ;
#9350 = CIRCLE ( 'NONE', #1308, 4.600000000000006750 ) ;
#9351 = LINE ( 'NONE', #3540, #10459 ) ;
#9352 = CARTESIAN_POINT ( 'NONE',  ( -102.5926225674731853, 102.8748711238780373, 20.00000000000000355 ) ) ;
#9353 = LINE ( 'NONE', #10384, #7233 ) ;
#9354 = VERTEX_POINT ( 'NONE', #7133 ) ;
#9355 = EDGE_CURVE ( 'NONE', #6374, #15744, #8629, .T. ) ;
#9356 = LINE ( 'NONE', #843, #5174 ) ;
#9357 = AXIS2_PLACEMENT_3D ( 'NONE', #14148, #18364, #18459 ) ;
#9358 = VECTOR ( 'NONE', #10475, 1000.000000000000000 ) ;
#9359 = VECTOR ( 'NONE', #5224, 1000.000000000000000 ) ;
#9360 = CARTESIAN_POINT ( 'NONE',  ( 98.04320049944426785, 84.22855780814606419, 62.50000000000001421 ) ) ;
#9361 = EDGE_LOOP ( 'NONE', ( #17811, #10538, #2670, #15288 ) ) ;
#9362 = CARTESIAN_POINT ( 'NONE',  ( -30.06971094502080177, -91.24992749556385263, -9.348345296714480668 ) ) ;
#9363 = DIRECTION ( 'NONE',  ( 0.000000000000000000, 0.000000000000000000, 1.000000000000000000 ) ) ;
#9364 = EDGE_LOOP ( 'NONE', ( #7833, #5892, #602 ) ) ;
#9365 = ADVANCED_FACE ( 'NONE', ( #1605 ), #4322, .F. ) ;
#9366 = VERTEX_POINT ( 'NONE', #15741 ) ;
#9367 = CIRCLE ( 'NONE', #110, 6.500000000000039968 ) ;
#9368 = VECTOR ( 'NONE', #7998, 1000.000000000000114 ) ;
#9369 = CARTESIAN_POINT ( 'NONE',  ( -71.24615306438106188, 35.13374195456378146, -167.1454815528550739 ) ) ;
#9370 = DIRECTION ( 'NONE',  ( 0.000000000000000000, 0.000000000000000000, 1.000000000000000000 ) ) ;
#9371 = DIRECTION ( 'NONE',  ( -0.000000000000000000, -0.000000000000000000, -1.000000000000000000 ) ) ;
#9372 = CARTESIAN_POINT ( 'NONE',  ( -102.4618227840623774, -111.0842361345572158, -57.00000000000000000 ) ) ;
#9373 = DIRECTION ( 'NONE',  ( -1.000000000000000000, 0.000000000000000000, -6.950654929607132427E-15 ) ) ;
#9374 = CARTESIAN_POINT ( 'NONE',  ( 0.5805565836007609004, 7.505553499465141165, -1.387778780781445676E-14 ) ) ;
#9375 = ORIENTED_EDGE ( 'NONE', *, *, #8615, .F. ) ;
#9376 = EDGE_CURVE ( 'NONE', #7034, #7430, #2923, .T. ) ;
#9377 = DIRECTION ( 'NONE',  ( -5.204170427930409450E-16, 0.000000000000000000, 1.000000000000000000 ) ) ;
#9378 = DIRECTION ( 'NONE',  ( 0.000000000000000000, 0.000000000000000000, 1.000000000000000000 ) ) ;
#9379 = CARTESIAN_POINT ( 'NONE',  ( -107.5926225674731853, 107.8748711238780373, -25.00000000000000000 ) ) ;
#9380 = ADVANCED_FACE ( 'NONE', ( #3011 ), #8721, .T. ) ;
#9381 = DIRECTION ( 'NONE',  ( -6.950654929607131638E-15, 0.000000000000000000, 1.000000000000000000 ) ) ;
#9382 = ORIENTED_EDGE ( 'NONE', *, *, #10507, .T. ) ;
#9383 = CARTESIAN_POINT ( 'NONE',  ( -71.24615306438074924, 107.3903729045637476, 15.00000000000006928 ) ) ;
#9384 = ORIENTED_EDGE ( 'NONE', *, *, #7616, .T. ) ;
#9385 = ADVANCED_FACE ( 'NONE', ( #10362 ), #1888, .F. ) ;
#9386 = VECTOR ( 'NONE', #15602, 999.9999999999998863 ) ;
#9387 = PLANE ( 'NONE',  #2030 ) ;
#9389 = ORIENTED_EDGE ( 'NONE', *, *, #2073, .F. ) ;
#9388 = AXIS2_PLACEMENT_3D ( 'NONE', #9462, #6657, #3939 ) ;
#9390 = EDGE_CURVE ( 'NONE', #2581, #18214, #13033, .T. ) ;
#9391 = ADVANCED_FACE ( 'NONE', ( #3100 ), #8814, .F. ) ;
#9392 = ORIENTED_EDGE ( 'NONE', *, *, #4698, .T. ) ;
#9393 = AXIS2_PLACEMENT_3D ( 'NONE', #8274, #11363, #11276 ) ;
#9394 = EDGE_CURVE ( 'NONE', #4629, #17860, #6154, .T. ) ;
#9395 = SURFACE_STYLE_FILL_AREA ( #9206 ) ;
#9396 = EDGE_CURVE ( 'NONE', #7586, #16233, #15052, .T. ) ;
#9397 = CARTESIAN_POINT ( 'NONE',  ( -69.56651066787533466, 84.80960611389535586, 15.00000000000006928 ) ) ;
#9398 = CARTESIAN_POINT ( 'NONE',  ( -97.59262256747319952, 61.64996188551983636, -25.00000000000000000 ) ) ;
#9399 = VECTOR ( 'NONE', #6430, 999.9999999999998863 ) ;
#9400 = VERTEX_POINT ( 'NONE', #4671 ) ;
#9401 = VECTOR ( 'NONE', #16772, 1000.000000000000000 ) ;
#9402 = AXIS2_PLACEMENT_3D ( 'NONE', #2139, #17941, #17563 ) ;
#9403 = CYLINDRICAL_SURFACE ( 'NONE', #13783, 10.24900000000000766 ) ;
#9404 = CARTESIAN_POINT ( 'NONE',  ( -92.59262256747319952, 57.88796029049329661, 26.35917033480641436 ) ) ;
#9405 = ORIENTED_EDGE ( 'NONE', *, *, #9069, .T. ) ;
#9406 = ADVANCED_FACE ( 'NONE', ( #2243 ), #14777, .T. ) ;
#9407 = CARTESIAN_POINT ( 'NONE',  ( -71.24615306438080609, 106.5015021652292404, 15.00000000000006928 ) ) ;
#9408 = LINE ( 'NONE', #880, #11696 ) ;
#9409 = ORIENTED_EDGE ( 'NONE', *, *, #13045, .F. ) ;
#9410 = DIRECTION ( 'NONE',  ( 0.000000000000000000, 1.000000000000000000, 0.000000000000000000 ) ) ;
#9411 = CYLINDRICAL_SURFACE ( 'NONE', #9932, 4.599999999999992539 ) ;
#9412 = AXIS2_PLACEMENT_3D ( 'NONE', #14445, #10048, #11549 ) ;
#9413 = LINE ( 'NONE', #17816, #1361 ) ;
#9414 = AXIS2_PLACEMENT_3D ( 'NONE', #5399, #8406, #4289 ) ;
#9415 = CARTESIAN_POINT ( 'NONE',  ( -76.78641432137852973, -94.06000857856476216, -44.58117269483251022 ) ) ;
#9416 = VECTOR ( 'NONE', #13374, 1000.000000000000000 ) ;
#9417 = ORIENTED_EDGE ( 'NONE', *, *, #6210, .T. ) ;
#9418 = AXIS2_PLACEMENT_3D ( 'NONE', #18236, #5598, #16923 ) ;
#9419 = EDGE_LOOP ( 'NONE', ( #8344, #6101, #7401, #13229 ) ) ;
#9420 = VERTEX_POINT ( 'NONE', #11878 ) ;
#9421 = CARTESIAN_POINT ( 'NONE',  ( 124.5381772159375942, -111.0842361345572158, 57.00000000000000000 ) ) ;
#9422 = DIRECTION ( 'NONE',  ( 0.000000000000000000, 0.000000000000000000, 1.000000000000000000 ) ) ;
#9423 = ORIENTED_EDGE ( 'NONE', *, *, #11329, .F. ) ;
#9424 = CARTESIAN_POINT ( 'NONE',  ( -75.72335493167709330, 106.9211863004614997, -28.00000000000000355 ) ) ;
#9425 = CARTESIAN_POINT ( 'NONE',  ( -4.730921629999971678, 17.21234141005219698, 44.69891962609317204 ) ) ;
#9426 = DIRECTION ( 'NONE',  ( 0.000000000000000000, 0.000000000000000000, 1.000000000000000000 ) ) ;
#9427 = ORIENTED_EDGE ( 'NONE', *, *, #10135, .F. ) ;
#9428 = DIRECTION ( 'NONE',  ( 0.000000000000000000, 0.000000000000000000, 1.000000000000000000 ) ) ;
#9429 = DIRECTION ( 'NONE',  ( 1.000000000000000000, 0.000000000000000000, 3.771137991253934490E-16 ) ) ;
#9430 = FILL_AREA_STYLE_COLOUR ( '', #3156 ) ;
#9431 = VECTOR ( 'NONE', #11117, 1000.000000000000114 ) ;
#9432 = CARTESIAN_POINT ( 'NONE',  ( -57.08002265617300708, 84.22855780814606419, -167.1454815528550739 ) ) ;
#9433 = ORIENTED_EDGE ( 'NONE', *, *, #16448, .F. ) ;
#9434 = CARTESIAN_POINT ( 'NONE',  ( -68.99615306438094819, 51.66063823166267355, -15.00000000000001421 ) ) ;
#9435 = CARTESIAN_POINT ( 'NONE',  ( -68.99615306438083451, 99.39938383813029077, -167.1454815528550739 ) ) ;
#9436 = ORIENTED_EDGE ( 'NONE', *, *, #12596, .F. ) ;
#9437 = DIRECTION ( 'NONE',  ( 0.000000000000000000, 0.000000000000000000, 1.000000000000000000 ) ) ;
#9438 = CARTESIAN_POINT ( 'NONE',  ( -36.62711323603792124, 79.27386099610184544, 56.86433512711490579 ) ) ;
#9439 = VERTEX_POINT ( 'NONE', #552 ) ;
#9440 = VERTEX_POINT ( 'NONE', #16446 ) ;
#9441 = APPLICATION_CONTEXT ( 'automotive_design' ) ;
#9442 = DIRECTION ( 'NONE',  ( 0.000000000000000000, 0.000000000000000000, 1.000000000000000000 ) ) ;
#9443 = ORIENTED_EDGE ( 'NONE', *, *, #4024, .F. ) ;
#9444 = DIRECTION ( 'NONE',  ( -5.204170427930409450E-16, 0.000000000000000000, 1.000000000000000000 ) ) ;
#9445 = DIRECTION ( 'NONE',  ( -0.9396926207859157554, 0.3420201433256481738, -4.890320548438487362E-16 ) ) ;
#9446 = LINE ( 'NONE', #10746, #2493 ) ;
#9447 = DIRECTION ( 'NONE',  ( 0.000000000000000000, 0.000000000000000000, -1.000000000000000000 ) ) ;
#9448 = DIRECTION ( 'NONE',  ( 0.000000000000000000, 0.000000000000000000, -1.000000000000000000 ) ) ;
#9449 = CARTESIAN_POINT ( 'NONE',  ( -47.76080550507955280, 75.89776002577458769, -167.1454815528550739 ) ) ;
#9450 = EDGE_LOOP ( 'NONE', ( #18177, #7179, #7768, #12465, #2275, #14563 ) ) ;
#9451 = LINE ( 'NONE', #3466, #16821 ) ;
#9452 = DIRECTION ( 'NONE',  ( 0.000000000000000000, 0.000000000000000000, 1.000000000000000000 ) ) ;
#9453 = ORIENTED_EDGE ( 'NONE', *, *, #468, .F. ) ;
#9454 = EDGE_CURVE ( 'NONE', #15032, #15460, #16161, .T. ) ;
#9455 = CARTESIAN_POINT ( 'NONE',  ( -26.13860949178274851, -94.06000665574431707, -6.066633903742957301 ) ) ;
#9456 = CARTESIAN_POINT ( 'NONE',  ( -71.24615306438097662, 56.23601976522923707, 15.00000000000006928 ) ) ;
#9457 = VERTEX_POINT ( 'NONE', #4853 ) ;
#9458 = ORIENTED_EDGE ( 'NONE', *, *, #17048, .F. ) ;
#9459 = ORIENTED_EDGE ( 'NONE', *, *, #13268, .F. ) ;
#9460 = DIRECTION ( 'NONE',  ( 1.156482317317869999E-16, 0.000000000000000000, 1.000000000000000000 ) ) ;
#9461 = PLANE ( 'NONE',  #5452 ) ;
#9462 = CARTESIAN_POINT ( 'NONE',  ( -127.5926225674731711, 57.88796029049329661, -26.35917033480641436 ) ) ;
#9463 = CARTESIAN_POINT ( 'NONE',  ( -71.24615306438101925, 25.70896400456379283, 15.00000000000006928 ) ) ;
#9464 = FACE_OUTER_BOUND ( 'NONE', #17773, .T. ) ;
#9465 = VERTEX_POINT ( 'NONE', #12254 ) ;
#9466 = DIRECTION ( 'NONE',  ( -0.000000000000000000, -0.000000000000000000, -1.000000000000000000 ) ) ;
#9467 = DIRECTION ( 'NONE',  ( -0.000000000000000000, 1.000000000000000000, -0.000000000000000000 ) ) ;
#9469 = ORIENTED_EDGE ( 'NONE', *, *, #586, .T. ) ;
#9468 = DIRECTION ( 'NONE',  ( 0.000000000000000000, 0.000000000000000000, -1.000000000000000000 ) ) ;
#9470 = CARTESIAN_POINT ( 'NONE',  ( -97.59262256747318531, 54.12595869546677818, 25.00000000000000000 ) ) ;
#9471 = PLANE ( 'NONE',  #14631 ) ;
#9472 = ORIENTED_EDGE ( 'NONE', *, *, #2010, .F. ) ;
#9473 = CARTESIAN_POINT ( 'NONE',  ( -68.99615306438086293, 89.97460588813027016, -167.1454815528550739 ) ) ;
#9474 = ORIENTED_EDGE ( 'NONE', *, *, #2248, .T. ) ;
#9475 = ORIENTED_EDGE ( 'NONE', *, *, #15355, .T. ) ;
#9476 = ADVANCED_FACE ( 'NONE', ( #13662 ), #12073, .T. ) ;
#9477 = CARTESIAN_POINT ( 'NONE',  ( -127.5926225674731711, 57.88796029049329661, -30.35917033480640370 ) ) ;
#9478 = CARTESIAN_POINT ( 'NONE',  ( -71.24615306438117557, 5.970537365229261262, -167.1454815528550739 ) ) ;
#9479 = EDGE_LOOP ( 'NONE', ( #11385, #3787, #14953, #15173 ) ) ;
#9480 = PRODUCT_CONTEXT ( 'NONE', #3453, 'mechanical' ) ;
#9481 = DIRECTION ( 'NONE',  ( 0.000000000000000000, 5.551115123125748189E-17, 1.000000000000000000 ) ) ;
#9482 = DIRECTION ( 'NONE',  ( 0.000000000000000000, 0.000000000000000000, 1.000000000000000000 ) ) ;
#9483 = ORIENTED_EDGE ( 'NONE', *, *, #7082, .T. ) ;
#9484 = LINE ( 'NONE', #6482, #17938 ) ;
#9485 = CARTESIAN_POINT ( 'NONE',  ( -57.08002265617300708, 84.22855780814606419, 15.00000000000006928 ) ) ;
#9486 = DIRECTION ( 'NONE',  ( 0.000000000000000000, 0.000000000000000000, 1.000000000000000000 ) ) ;
#9487 = EDGE_CURVE ( 'NONE', #17232, #9825, #9353, .T. ) ;
#9488 = ORIENTED_EDGE ( 'NONE', *, *, #7030, .T. ) ;
#9489 = EDGE_CURVE ( 'NONE', #8001, #6374, #14397, .T. ) ;
#9490 = DIRECTION ( 'NONE',  ( 0.000000000000000000, 0.000000000000000000, 1.000000000000000000 ) ) ;
#9491 = CARTESIAN_POINT ( 'NONE',  ( -67.59262256747319952, 106.8071537307723133, 25.00000000000000355 ) ) ;
#9492 = EDGE_CURVE ( 'NONE', #8164, #6219, #653, .T. ) ;
#9493 = DIRECTION ( 'NONE',  ( -1.000000000000000000, 0.000000000000000000, 0.000000000000000000 ) ) ;
#9494 = FACE_OUTER_BOUND ( 'NONE', #8392, .T. ) ;
#9495 = ORIENTED_EDGE ( 'NONE', *, *, #14808, .F. ) ;
#9496 = VECTOR ( 'NONE', #12573, 1000.000000000000000 ) ;
#9497 = ADVANCED_FACE ( 'NONE', ( #4956 ), #10749, .T. ) ;
#9498 = ADVANCED_FACE ( 'NONE', ( #7585 ), #13567, .F. ) ;
#9499 = ADVANCED_FACE ( 'NONE', ( #10670 ), #13298, .F. ) ;
#9500 = VERTEX_POINT ( 'NONE', #16167 ) ;
#9501 = DIRECTION ( 'NONE',  ( 1.000000000000000000, 0.000000000000000000, 0.000000000000000000 ) ) ;
#9502 = DIRECTION ( 'NONE',  ( -1.000000000000000000, 0.000000000000000000, -9.912705577010330480E-16 ) ) ;
#9503 = ORIENTED_EDGE ( 'NONE', *, *, #5271, .T. ) ;
#9504 = ADVANCED_FACE ( 'NONE', ( #3358 ), #14861, .T. ) ;
#9505 = CARTESIAN_POINT ( 'NONE',  ( -76.37409655828265898, -96.08423613455721579, -8.001217251689905290E-13 ) ) ;
#9506 = CARTESIAN_POINT ( 'NONE',  ( -76.81489084760232799, 76.92303621577350725, 64.21479655795450014 ) ) ;
#9507 = CARTESIAN_POINT ( 'NONE',  ( -68.99615306438106188, 24.00116023813026445, -15.00000000000001421 ) ) ;
#9508 = DIRECTION ( 'NONE',  ( 0.000000000000000000, 0.000000000000000000, -1.000000000000000000 ) ) ;
#9509 = ORIENTED_EDGE ( 'NONE', *, *, #4458, .T. ) ;
#9510 = CYLINDRICAL_SURFACE ( 'NONE', #4783, 4.599999999999992539 ) ;
#9511 = DIRECTION ( 'NONE',  ( -1.000000000000000000, -3.016910393003138520E-15, 0.000000000000000000 ) ) ;
#9512 = AXIS2_PLACEMENT_3D ( 'NONE', #7958, #17957, #13669 ) ;
#9513 = PLANE ( 'NONE',  #16486 ) ;
#9514 = CARTESIAN_POINT ( 'NONE',  ( -18.61292065092662185, 46.98476669316325172, 29.30995736292643628 ) ) ;
#9515 = ORIENTED_EDGE ( 'NONE', *, *, #7780, .F. ) ;
#9516 = EDGE_CURVE ( 'NONE', #8485, #4505, #9315, .T. ) ;
#9517 = CARTESIAN_POINT ( 'NONE',  ( -71.24615306438091977, 75.97444640456376419, -167.1454815528550739 ) ) ;
#9518 = DIRECTION ( 'NONE',  ( 1.047634945911799279E-14, 0.000000000000000000, -1.000000000000000000 ) ) ;
#9519 = ADVANCED_FACE ( 'NONE', ( #13471 ), #6343, .T. ) ;
#9520 = ORIENTED_EDGE ( 'NONE', *, *, #16462, .F. ) ;
#9521 = CARTESIAN_POINT ( 'NONE',  ( -68.99615306438077766, 114.4924912316626688, -167.1454815528550739 ) ) ;
#9522 = CARTESIAN_POINT ( 'NONE',  ( -36.89537005233415812, 78.27079066365615745, 57.91772688325330876 ) ) ;
#9523 = ORIENTED_EDGE ( 'NONE', *, *, #2535, .F. ) ;
#9524 = ORIENTED_EDGE ( 'NONE', *, *, #7229, .F. ) ;
#9525 = AXIS2_PLACEMENT_3D ( 'NONE', #12798, #5578, #8297 ) ;
#9526 = CARTESIAN_POINT ( 'NONE',  ( -92.59262256747318531, 0.3328663868096687350, 25.00000000000000000 ) ) ;
#9527 = ORIENTED_EDGE ( 'NONE', *, *, #16448, .T. ) ;
#9528 = CYLINDRICAL_SURFACE ( 'NONE', #9717, 42.49926016644912607 ) ;
#9529 = CARTESIAN_POINT ( 'NONE',  ( -100.4870060002411805, -151.5628872026273086, -57.00000000000000000 ) ) ;
#9530 = CARTESIAN_POINT ( 'NONE',  ( -67.15995696847650720, 60.73698500726539606, -28.00000000000000355 ) ) ;
#9531 = CARTESIAN_POINT ( 'NONE',  ( -57.08002265617300708, 84.22855780814606419, -167.1454815528550739 ) ) ;
#9532 = CARTESIAN_POINT ( 'NONE',  ( 0.06682554136337354178, 6.264794173742258998, 2.149058192116914068 ) ) ;
#9533 = CARTESIAN_POINT ( 'NONE',  ( -70.71978124295696944, -141.5628872026273086, 5.204170427930421283E-15 ) ) ;
#9534 = DIRECTION ( 'NONE',  ( -5.204170427930409450E-16, 0.000000000000000000, 1.000000000000000000 ) ) ;
#9535 = PRODUCT_DEFINITION_SHAPE ( 'NONE', 'NONE',  #7385 ) ;
#9536 = ORIENTED_EDGE ( 'NONE', *, *, #2732, .T. ) ;
#9537 = EDGE_CURVE ( 'NONE', #2450, #7505, #7033, .T. ) ;
#9538 = CARTESIAN_POINT ( 'NONE',  ( -68.99615306438111872, 11.43478963813029914, -167.1454815528550739 ) ) ;
#9539 = CARTESIAN_POINT ( 'NONE',  ( -71.24615306438097662, 63.40807580456375803, 15.00000000000006928 ) ) ;
#9540 = VECTOR ( 'NONE', #108, 1000.000000000000114 ) ;
#9541 = ORIENTED_EDGE ( 'NONE', *, *, #822, .F. ) ;
#9542 = CARTESIAN_POINT ( 'NONE',  ( -68.99615306438070661, 133.9569029881302811, -15.00000000000001421 ) ) ;
#9543 = DIRECTION ( 'NONE',  ( 0.000000000000000000, 0.000000000000000000, -1.000000000000000000 ) ) ;
#9544 = VERTEX_POINT ( 'NONE', #13945 ) ;
#9545 = ORIENTED_EDGE ( 'NONE', *, *, #4926, .F. ) ;
#9546 = DIRECTION ( 'NONE',  ( 0.000000000000000000, 0.000000000000000000, 1.000000000000000000 ) ) ;
#9547 = CARTESIAN_POINT ( 'NONE',  ( 103.5381772159376084, -111.0842361345572158, 57.00000000000000000 ) ) ;
#9548 = CIRCLE ( 'NONE', #16105, 11.04359719766050141 ) ;
#9549 = LINE ( 'NONE', #6550, #15359 ) ;
#9550 = ADVANCED_FACE ( 'NONE', ( #10952 ), #17948, .T. ) ;
#9551 = CARTESIAN_POINT ( 'NONE',  ( -71.24615306438100504, 53.98329785456373742, -167.1454815528550739 ) ) ;
#9552 = FACE_OUTER_BOUND ( 'NONE', #10535, .T. ) ;
#9553 = VECTOR ( 'NONE', #11161, 1000.000000000000000 ) ;
#9554 = DIRECTION ( 'NONE',  ( 1.156482317317869999E-16, 0.000000000000000000, 1.000000000000000000 ) ) ;
#9555 = VERTEX_POINT ( 'NONE', #15439 ) ;
#9556 = CARTESIAN_POINT ( 'NONE',  ( -65.94558993203320085, 89.37090336996871542, -15.00000000000001421 ) ) ;
#9557 = CARTESIAN_POINT ( 'NONE',  ( 0.000000000000000000, 2.220446049250313081E-16, 4.000000000000024869 ) ) ;
#9560 = EDGE_CURVE ( 'NONE', #3211, #3179, #2428, .T. ) ;
#9559 = VERTEX_POINT ( 'NONE', #6737 ) ;
#9558 = LINE ( 'NONE', #6665, #5767 ) ;
#9561 = PLANE ( 'NONE',  #17689 ) ;
#9562 = DIRECTION ( 'NONE',  ( 0.3420201433256546686, -0.9396926207859135349, 0.000000000000000000 ) ) ;
#9563 = ORIENTED_EDGE ( 'NONE', *, *, #7909, .F. ) ;
#9564 = VERTEX_POINT ( 'NONE', #8236 ) ;
#9565 = VECTOR ( 'NONE', #7230, 1000.000000000000000 ) ;
#9566 = CIRCLE ( 'NONE', #15242, 3.999999999999989786 ) ;
#9567 = AXIS2_PLACEMENT_3D ( 'NONE', #15894, #17378, #10284 ) ;
#9568 = ORIENTED_EDGE ( 'NONE', *, *, #727, .F. ) ;
#9569 = CARTESIAN_POINT ( 'NONE',  ( -64.58002265617299997, 84.22855780814606419, 15.00000000000006573 ) ) ;
#9570 = DIRECTION ( 'NONE',  ( 0.9396926207859185309, 0.3420201433256406798, -1.086737899653001478E-16 ) ) ;
#9571 = DIRECTION ( 'NONE',  ( 0.000000000000000000, -1.000000000000000000, 0.000000000000000000 ) ) ;
#9572 = ORIENTED_EDGE ( 'NONE', *, *, #17022, .F. ) ;
#9573 = CIRCLE ( 'NONE', #1523, 4.599999999999992539 ) ;
#9574 = CARTESIAN_POINT ( 'NONE',  ( 4.699999999999995737, -5.629165124598954684, 3.250000000000013323 ) ) ;
#9575 = AXIS2_PLACEMENT_3D ( 'NONE', #18055, #8139, #844 ) ;
#9576 = CARTESIAN_POINT ( 'NONE',  ( -71.24615306438080609, 103.3599095152292193, -167.1454815528550739 ) ) ;
#9577 = ORIENTED_EDGE ( 'NONE', *, *, #416, .F. ) ;
#9578 =( NAMED_UNIT ( * ) PLANE_ANGLE_UNIT ( ) SI_UNIT ( $, .RADIAN. ) );
#9579 = CARTESIAN_POINT ( 'NONE',  ( -68.99615306438093398, 64.84186468813030046, -15.00000000000001421 ) ) ;
#9580 = DIRECTION ( 'NONE',  ( 1.000000000000000000, 0.000000000000000000, 0.000000000000000000 ) ) ;
#9581 = VECTOR ( 'NONE', #14013, 1000.000000000000114 ) ;
#9582 = VERTEX_POINT ( 'NONE', #14134 ) ;
#9583 = CIRCLE ( 'NONE', #16135, 4.599999999999992539 ) ;
#9584 = CARTESIAN_POINT ( 'NONE',  ( -70.06856178257680767, 110.5691553257988460, -22.35917033480641791 ) ) ;
#9585 = FACE_OUTER_BOUND ( 'NONE', #12427, .T. ) ;
#9586 = EDGE_CURVE ( 'NONE', #11230, #5649, #12456, .T. ) ;
#9587 = CARTESIAN_POINT ( 'NONE',  ( -71.24615306438101925, 47.70011255456375210, -15.00000000000001421 ) ) ;
#9588 = VECTOR ( 'NONE', #403, 1000.000000000000114 ) ;
#9589 = DIRECTION ( 'NONE',  ( 0.000000000000000000, 1.000000000000000000, 0.000000000000000000 ) ) ;
#9590 = ORIENTED_EDGE ( 'NONE', *, *, #11566, .F. ) ;
#9591 = VECTOR ( 'NONE', #14351, 1000.000000000000000 ) ;
#9592 = CIRCLE ( 'NONE', #11697, 21.04359719766049608 ) ;
#9593 = EDGE_CURVE ( 'NONE', #10434, #13327, #5523, .T. ) ;
#9594 = DIRECTION ( 'NONE',  ( 0.1309959539064320944, 0.9913829028484121286, 1.514972713530672604E-13 ) ) ;
#9595 = CARTESIAN_POINT ( 'NONE',  ( -42.53669312409158465, -111.0842361345572158, 5.204170427930421283E-15 ) ) ;
#9596 = EDGE_CURVE ( 'NONE', #800, #7936, #11142, .T. ) ;
#9597 = ORIENTED_EDGE ( 'NONE', *, *, #1721, .F. ) ;
#9598 = FACE_OUTER_BOUND ( 'NONE', #6818, .T. ) ;
#9599 = PLANE ( 'NONE',  #10431 ) ;
#9600 = FACE_OUTER_BOUND ( 'NONE', #10463, .T. ) ;
#9601 = DIRECTION ( 'NONE',  ( -1.000000000000000000, 0.000000000000000000, 0.000000000000000000 ) ) ;
#9602 = VERTEX_POINT ( 'NONE', #8425 ) ;
#9603 = CIRCLE ( 'NONE', #8726, 5.000000000000000000 ) ;
#9604 = LINE ( 'NONE', #12523, #17631 ) ;
#9605 = DIRECTION ( 'NONE',  ( 1.000000000000000000, 0.000000000000000000, 3.771137991253934490E-16 ) ) ;
#9606 = LINE ( 'NONE', #15504, #2446 ) ;
#9607 = CARTESIAN_POINT ( 'NONE',  ( -4.030484272568896742, 33.41412046829307059, 37.23164655599730821 ) ) ;
#9608 = EDGE_LOOP ( 'NONE', ( #5049, #12393, #18117, #7447 ) ) ;
#9609 = EDGE_CURVE ( 'NONE', #10351, #16485, #8449, .T. ) ;
#9610 = EDGE_CURVE ( 'NONE', #6984, #425, #12357, .T. ) ;
#9611 = VECTOR ( 'NONE', #4395, 1000.000000000000000 ) ;
#9612 = VECTOR ( 'NONE', #12383, 1000.000000000000000 ) ;
#9613 = DIRECTION ( 'NONE',  ( 0.3420201433256724322, 0.9396926207859070956, -0.000000000000000000 ) ) ;
#9614 = CARTESIAN_POINT ( 'NONE',  ( -60.71745612804077297, -91.12516132330414109, 39.81918451580458651 ) ) ;
#9615 = CARTESIAN_POINT ( 'NONE',  ( -57.08002265617300708, 84.22855780814606419, 28.00000000000000355 ) ) ;
#9616 = CARTESIAN_POINT ( 'NONE',  ( -36.53717731224358545, 79.64648582715004466, 68.45756564509078146 ) ) ;
#9617 = ORIENTED_EDGE ( 'NONE', *, *, #6814, .F. ) ;
#9618 = ORIENTED_EDGE ( 'NONE', *, *, #9148, .F. ) ;
#9619 = EDGE_CURVE ( 'NONE', #1231, #6109, #2457, .T. ) ;
#9620 = AXIS2_PLACEMENT_3D ( 'NONE', #13155, #14639, #8587 ) ;
#9621 = EDGE_CURVE ( 'NONE', #4482, #13472, #2714, .T. ) ;
#9622 = DIRECTION ( 'NONE',  ( 4.124608743189000987E-16, -1.000000000000000000, 0.000000000000000000 ) ) ;
#9623 = ORIENTED_EDGE ( 'NONE', *, *, #9851, .T. ) ;
#9624 = AXIS2_PLACEMENT_3D ( 'NONE', #12026, #12310, #10805 ) ;
#9625 = VECTOR ( 'NONE', #15342, 1000.000000000000000 ) ;
#9626 = EDGE_CURVE ( 'NONE', #7586, #513, #1325, .T. ) ;
#9627 = CARTESIAN_POINT ( 'NONE',  ( -66.56181127008836995, 56.43195750230852070, 24.56257327959996317 ) ) ;
#9628 = PLANE ( 'NONE',  #4567 ) ;
#9629 = EDGE_CURVE ( 'NONE', #15808, #103, #13848, .T. ) ;
#9630 = DIRECTION ( 'NONE',  ( -0.9396926207858995461, 0.3420201433256928603, 1.086737899652979538E-16 ) ) ;
#9631 = ORIENTED_EDGE ( 'NONE', *, *, #10945, .F. ) ;
#9632 = CARTESIAN_POINT ( 'NONE',  ( -48.98198201484814263, 93.75072866207695199, -15.00000000000001421 ) ) ;
#9633 = LINE ( 'NONE', #8234, #11224 ) ;
#9634 = FACE_OUTER_BOUND ( 'NONE', #5968, .T. ) ;
#9635 = DIRECTION ( 'NONE',  ( -1.000000000000000000, -2.062304371594500247E-16, -0.000000000000000000 ) ) ;
#9636 = ORIENTED_EDGE ( 'NONE', *, *, #820, .F. ) ;
#9637 = EDGE_CURVE ( 'NONE', #15366, #15625, #3645, .T. ) ;
#9638 = CONICAL_SURFACE ( 'NONE', #13232, 3.999999999999989786, 1.029744258676652091 ) ;
#9639 = LINE ( 'NONE', #16638, #4211 ) ;
#9640 = VERTEX_POINT ( 'NONE', #16635 ) ;
#9641 = CIRCLE ( 'NONE', #10238, 45.40389983439752086 ) ;
#9642 = PLANE ( 'NONE',  #17777 ) ;
#9643 = AXIS2_PLACEMENT_3D ( 'NONE', #16025, #14802, #15166 ) ;
#9644 = CARTESIAN_POINT ( 'NONE',  ( 103.5381772159376084, -151.5628872026272802, -36.00000000000000000 ) ) ;
#9645 = ORIENTED_EDGE ( 'NONE', *, *, #795, .F. ) ;
#9646 = ORIENTED_EDGE ( 'NONE', *, *, #7764, .T. ) ;
#9647 = ORIENTED_EDGE ( 'NONE', *, *, #9069, .F. ) ;
#9648 = AXIS2_PLACEMENT_3D ( 'NONE', #4686, #2161, #16466 ) ;
#9649 = FACE_OUTER_BOUND ( 'NONE', #3392, .T. ) ;
#9650 = CARTESIAN_POINT ( 'NONE',  ( -71.24615306438101925, 41.41692725456378810, -15.00000000000001421 ) ) ;
#9651 = CARTESIAN_POINT ( 'NONE',  ( -123.4618227840623632, -111.0842361345572158, 18.23991632971911869 ) ) ;
#9652 = DIRECTION ( 'NONE',  ( -0.000000000000000000, -0.000000000000000000, -1.000000000000000000 ) ) ;
#9653 = VECTOR ( 'NONE', #2420, 1000.000000000000000 ) ;
#9654 = LINE ( 'NONE', #11536, #18234 ) ;
#9655 = AXIS2_PLACEMENT_3D ( 'NONE', #3190, #117, #11805 ) ;
#9656 = AXIS2_PLACEMENT_3D ( 'NONE', #3820, #12243, #2042 ) ;
#9657 = CARTESIAN_POINT ( 'NONE',  ( -46.03642545851250389, 84.22855780814606419, 68.73600986863397111 ) ) ;
#9658 = ORIENTED_EDGE ( 'NONE', *, *, #5843, .T. ) ;
#9659 = DIRECTION ( 'NONE',  ( 0.000000000000000000, 0.000000000000000000, 1.000000000000000000 ) ) ;
#9660 = DIRECTION ( 'NONE',  ( 1.000000000000000000, 0.000000000000000000, 0.000000000000000000 ) ) ;
#9662 = ORIENTED_EDGE ( 'NONE', *, *, #9560, .T. ) ;
#9661 = CARTESIAN_POINT ( 'NONE',  ( -77.78773836288226562, 87.99602245404173573, 69.00331597549191542 ) ) ;
#9663 = LINE ( 'NONE', #2842, #4569 ) ;
#9664 = DIRECTION ( 'NONE',  ( 0.000000000000000000, 0.000000000000000000, 1.000000000000000000 ) ) ;
#9665 = VERTEX_POINT ( 'NONE', #8323 ) ;
#9666 = VECTOR ( 'NONE', #3514, 1000.000000000000000 ) ;
#9667 = DIRECTION ( 'NONE',  ( 0.000000000000000000, 0.000000000000000000, 1.000000000000000000 ) ) ;
#9668 = VERTEX_POINT ( 'NONE', #6635 ) ;
#9669 =( GEOMETRIC_REPRESENTATION_CONTEXT ( 3 ) GLOBAL_UNCERTAINTY_ASSIGNED_CONTEXT ( ( #3473 ) ) GLOBAL_UNIT_ASSIGNED_CONTEXT ( ( #2021, #13439, #812 ) ) REPRESENTATION_CONTEXT ( 'NONE', 'WORKASPACE' ) );
#9670 = VECTOR ( 'NONE', #3825, 1000.000000000000000 ) ;
#9671 = VECTOR ( 'NONE', #10637, 1000.000000000000000 ) ;
#9672 = ORIENTED_EDGE ( 'NONE', *, *, #2, .T. ) ;
#9673 = CARTESIAN_POINT ( 'NONE',  ( -65.16279959635889441, 77.92691374209478283, -167.1454815528550739 ) ) ;
#9674 = DIRECTION ( 'NONE',  ( 0.000000000000000000, 1.000000000000000000, 0.000000000000000000 ) ) ;
#9675 = DIRECTION ( 'NONE',  ( -1.000000000000000000, 0.000000000000000000, 0.000000000000000000 ) ) ;
#9676 = VECTOR ( 'NONE', #57, 1000.000000000000000 ) ;
#9677 = ORIENTED_EDGE ( 'NONE', *, *, #3858, .T. ) ;
#9678 = SHAPE_DEFINITION_REPRESENTATION ( #6699, #17553 ) ;
#9679 = VERTEX_POINT ( 'NONE', #3923 ) ;
#9680 = CARTESIAN_POINT ( 'NONE',  ( -21.14627411319134254, 48.72449396156541468, -28.16502384431897710 ) ) ;
#9681 = DIRECTION ( 'NONE',  ( 0.000000000000000000, 0.000000000000000000, -1.000000000000000000 ) ) ;
#9682 = ORIENTED_EDGE ( 'NONE', *, *, #8992, .T. ) ;
#9683 = FILL_AREA_STYLE ('',( #13699 ) ) ;
#9684 = DIRECTION ( 'NONE',  ( 1.000000000000000000, 0.000000000000000000, 0.000000000000000000 ) ) ;
#9685 = CARTESIAN_POINT ( 'NONE',  ( -92.59262256747321373, 110.5691553257988460, -26.35917033480641436 ) ) ;
#9686 = VECTOR ( 'NONE', #9426, 1000.000000000000000 ) ;
#9687 = ORIENTED_EDGE ( 'NONE', *, *, #2048, .F. ) ;
#9688 = VECTOR ( 'NONE', #15930, 1000.000000000000114 ) ;
#9689 = DIRECTION ( 'NONE',  ( 1.156482317317869999E-16, 0.000000000000000000, 1.000000000000000000 ) ) ;
#9690 = LINE ( 'NONE', #5566, #3958 ) ;
#9691 = EDGE_LOOP ( 'NONE', ( #4975, #2188, #13311, #14063, #7339, #9762 ) ) ;
#9692 = DIRECTION ( 'NONE',  ( -0.1309959539066819501, 0.9913829028483791550, 0.000000000000000000 ) ) ;
#9693 =( REPRESENTATION_RELATIONSHIP ('NONE','NONE', #359, #5501 ) REPRESENTATION_RELATIONSHIP_WITH_TRANSFORMATION ( #14174 )SHAPE_REPRESENTATION_RELATIONSHIP( ) );
#9694 = VECTOR ( 'NONE', #2359, 1000.000000000000000 ) ;
#9695 = CARTESIAN_POINT ( 'NONE',  ( -66.51107682098671603, 56.41472097771080030, -24.67867649519316586 ) ) ;
#9696 = ORIENTED_EDGE ( 'NONE', *, *, #17709, .T. ) ;
#9697 = VECTOR ( 'NONE', #52, 1000.000000000000000 ) ;
#9698 = AXIS2_PLACEMENT_3D ( 'NONE', #8860, #1732, #13150 ) ;
#9699 = VECTOR ( 'NONE', #15815, 1000.000000000000000 ) ;
#9700 = DIRECTION ( 'NONE',  ( 0.000000000000000000, 0.000000000000000000, 1.000000000000000000 ) ) ;
#9701 = CARTESIAN_POINT ( 'NONE',  ( -71.24615306438076345, 125.3510580652292248, -15.00000000000001421 ) ) ;
#9702 = ORIENTED_EDGE ( 'NONE', *, *, #9487, .T. ) ;
#9703 = EDGE_CURVE ( 'NONE', #18220, #12020, #4119, .T. ) ;
#9704 = LINE ( 'NONE', #12428, #1198 ) ;
#9705 = LINE ( 'NONE', #1192, #12221 ) ;
#9706 = FACE_OUTER_BOUND ( 'NONE', #8025, .T. ) ;
#9707 = FACE_OUTER_BOUND ( 'NONE', #13787, .T. ) ;
#9708 = ORIENTED_EDGE ( 'NONE', *, *, #4359, .F. ) ;
#9709 = VECTOR ( 'NONE', #10894, 1000.000000000000000 ) ;
#9710 = DIRECTION ( 'NONE',  ( 1.000000000000000000, 0.000000000000000000, 0.000000000000000000 ) ) ;
#9711 = FACE_OUTER_BOUND ( 'NONE', #17656, .T. ) ;
#9712 = CARTESIAN_POINT ( 'NONE',  ( -5.674266893243433252, 18.91634531463802205, -44.04015471320351338 ) ) ;
#9713 = CARTESIAN_POINT ( 'NONE',  ( 7.760541235713054320, 14.88095002529105493, 45.61112162941545023 ) ) ;
#9714 = ORIENTED_EDGE ( 'NONE', *, *, #14729, .F. ) ;
#9715 = VECTOR ( 'NONE', #2201, 1000.000000000000000 ) ;
#9716 = AXIS2_PLACEMENT_3D ( 'NONE', #5417, #15438, #2623 ) ;
#9717 = AXIS2_PLACEMENT_3D ( 'NONE', #15231, #12745, #10268 ) ;
#9718 = DIRECTION ( 'NONE',  ( 0.000000000000000000, 1.000000000000000000, 0.000000000000000000 ) ) ;
#9719 = DIRECTION ( 'NONE',  ( 1.000000000000000000, 0.000000000000000000, 0.000000000000000000 ) ) ;
#9720 = EDGE_CURVE ( 'NONE', #7155, #16062, #3829, .T. ) ;
#9721 = EDGE_CURVE ( 'NONE', #7261, #17089, #2531, .T. ) ;
#9722 = CARTESIAN_POINT ( 'NONE',  ( -194.4437806548868934, -151.5628872026273086, -18.23991632971910803 ) ) ;
#9723 = CARTESIAN_POINT ( 'NONE',  ( -37.39921487797633404, 76.77809071147591169, 63.49146505177037625 ) ) ;
#9724 = ORIENTED_EDGE ( 'NONE', *, *, #9328, .F. ) ;
#9725 = VERTEX_POINT ( 'NONE', #5418 ) ;
#9726 = CARTESIAN_POINT ( 'NONE',  ( -71.24615306438086293, 101.1071876045637055, -167.1454815528550739 ) ) ;
#9727 = VECTOR ( 'NONE', #13951, 1000.000000000000000 ) ;
#9728 = ADVANCED_FACE ( 'NONE', ( #16834 ), #5877, .F. ) ;
#9729 = EDGE_CURVE ( 'NONE', #3050, #7136, #13223, .T. ) ;
#9730 = VECTOR ( 'NONE', #11859, 1000.000000000000114 ) ;
#9731 = DIRECTION ( 'NONE',  ( -1.000000000000000000, 0.000000000000000000, -6.950654929607132427E-15 ) ) ;
#9732 = CARTESIAN_POINT ( 'NONE',  ( -75.58239991587453233, 61.41969864223252529, 24.46191329895506783 ) ) ;
#9733 = CARTESIAN_POINT ( 'NONE',  ( -71.24615306438079188, 112.7846874652292399, 15.00000000000006928 ) ) ;
#9734 = ORIENTED_EDGE ( 'NONE', *, *, #8118, .F. ) ;
#9735 = DIRECTION ( 'NONE',  ( -4.124608743189000987E-16, 1.000000000000000000, 0.000000000000000000 ) ) ;
#9736 = DIRECTION ( 'NONE',  ( 1.000000000000000000, 0.000000000000000000, 0.000000000000000000 ) ) ;
#9737 = DIRECTION ( 'NONE',  ( -1.000000000000000000, -0.000000000000000000, -0.000000000000000000 ) ) ;
#9738 = CARTESIAN_POINT ( 'NONE',  ( -3.930119462002491844E-14, -96.08423613455721579, 5.654315315326165603 ) ) ;
#9739 = VERTEX_POINT ( 'NONE', #267 ) ;
#9740 = EDGE_CURVE ( 'NONE', #850, #18326, #15295, .T. ) ;
#9741 = DIRECTION ( 'NONE',  ( 1.000000000000000000, 0.000000000000000000, 0.000000000000000000 ) ) ;
#9742 = EDGE_CURVE ( 'NONE', #17074, #5963, #1675, .T. ) ;
#9743 = ORIENTED_EDGE ( 'NONE', *, *, #12747, .F. ) ;
#9744 = ADVANCED_FACE ( 'NONE', ( #15802 ), #1581, .T. ) ;
#9745 = CARTESIAN_POINT ( 'NONE',  ( -60.71187100093244737, 74.64462966772953223, 15.00000000000006928 ) ) ;
#9746 = VECTOR ( 'NONE', #5475, 1000.000000000000227 ) ;
#9747 = DIRECTION ( 'NONE',  ( 0.9396926207859171987, 0.3420201433256444545, 0.000000000000000000 ) ) ;
#9749 = ORIENTED_EDGE ( 'NONE', *, *, #18430, .T. ) ;
#9748 = AXIS2_PLACEMENT_3D ( 'NONE', #10779, #14977, #3764 ) ;
#9750 = EDGE_CURVE ( 'NONE', #9582, #14582, #941, .T. ) ;
#9751 = VERTEX_POINT ( 'NONE', #17114 ) ;
#9752 = ORIENTED_EDGE ( 'NONE', *, *, #15764, .F. ) ;
#9753 = EDGE_CURVE ( 'NONE', #16693, #13576, #12921, .T. ) ;
#9754 = ADVANCED_FACE ( 'NONE', ( #92 ), #10277, .T. ) ;
#9755 = EDGE_CURVE ( 'NONE', #18489, #16773, #11723, .T. ) ;
#9756 = DIRECTION ( 'NONE',  ( -1.000000000000000000, -0.000000000000000000, -0.000000000000000000 ) ) ;
#9757 = DIRECTION ( 'NONE',  ( -1.000000000000000000, 3.016910393003147592E-15, 0.000000000000000000 ) ) ;
#9758 = CARTESIAN_POINT ( 'NONE',  ( -57.08002265617300708, 84.22855780814606419, 28.00000000000000355 ) ) ;
#9759 = CARTESIAN_POINT ( 'NONE',  ( -68.99615306438091977, 76.79337943166271430, -15.00000000000001421 ) ) ;
#9760 = CARTESIAN_POINT ( 'NONE',  ( -71.24615306438076345, 122.2094654152292037, -15.00000000000001421 ) ) ;
#9761 = CARTESIAN_POINT ( 'NONE',  ( -68.99615306438099083, 49.13390143813028743, -15.00000000000001421 ) ) ;
#9762 = ORIENTED_EDGE ( 'NONE', *, *, #934, .F. ) ;
#9763 = DIRECTION ( 'NONE',  ( 1.000000000000000000, 0.000000000000000000, 3.771137991253923150E-16 ) ) ;
#9764 = EDGE_LOOP ( 'NONE', ( #462, #6473, #6700, #18122 ) ) ;
#9765 = DIRECTION ( 'NONE',  ( 1.000000000000000000, 0.000000000000000000, 0.000000000000000000 ) ) ;
#9766 = CARTESIAN_POINT ( 'NONE',  ( -107.5926225674731853, 110.5691553257988460, -30.38417033480641294 ) ) ;
#9767 = ORIENTED_EDGE ( 'NONE', *, *, #10844, .T. ) ;
#9768 = EDGE_CURVE ( 'NONE', #3038, #14123, #5605, .T. ) ;
#9769 = ORIENTED_EDGE ( 'NONE', *, *, #8349, .T. ) ;
#9770 = EDGE_CURVE ( 'NONE', #10136, #7810, #5787, .T. ) ;
#9771 = ORIENTED_EDGE ( 'NONE', *, *, #14954, .T. ) ;
#9772 = DIRECTION ( 'NONE',  ( 0.3420201433256686574, 0.9396926207859084279, -0.000000000000000000 ) ) ;
#9773 = DIRECTION ( 'NONE',  ( -1.000000000000000000, -0.000000000000000000, -0.000000000000000000 ) ) ;
#9774 = ORIENTED_EDGE ( 'NONE', *, *, #2145, .F. ) ;
#9775 = APPLICATION_PROTOCOL_DEFINITION ( 'draft international standard', 'automotive_design', 1998, #6933 ) ;
#9776 = CARTESIAN_POINT ( 'NONE',  ( -4.069817365965976208, 33.48920034010672708, -37.19988592485734102 ) ) ;
#9777 = CARTESIAN_POINT ( 'NONE',  ( -54.95363092160842911, 73.63336328296981037, 15.00000000000006928 ) ) ;
#9778 = ORIENTED_EDGE ( 'NONE', *, *, #13046, .T. ) ;
#9779 = LINE ( 'NONE', #1092, #12285 ) ;
#9780 = DIRECTION ( 'NONE',  ( -0.000000000000000000, -0.000000000000000000, -1.000000000000000000 ) ) ;
#9781 = DIRECTION ( 'NONE',  ( 1.000000000000000000, 2.062304371594500494E-16, 0.000000000000000000 ) ) ;
#9782 = ORIENTED_EDGE ( 'NONE', *, *, #7794, .T. ) ;
#9783 = CARTESIAN_POINT ( 'NONE',  ( -72.05036370780659638, 109.4994693637201664, -22.49689322592065466 ) ) ;
#9784 = DIRECTION ( 'NONE',  ( 0.000000000000000000, 0.000000000000000000, 1.000000000000000000 ) ) ;
#9785 = VERTEX_POINT ( 'NONE', #10183 ) ;
#9786 = EDGE_CURVE ( 'NONE', #13041, #115, #15629, .T. ) ;
#9787 = CARTESIAN_POINT ( 'NONE',  ( -71.24615306438080609, 116.8151508545637114, -167.1454815528550739 ) ) ;
#9788 = CARTESIAN_POINT ( 'NONE',  ( -107.5926225674731853, 110.5691553257988460, -26.35917033480641436 ) ) ;
#9789 = VERTEX_POINT ( 'NONE', #4393 ) ;
#9790 = ORIENTED_EDGE ( 'NONE', *, *, #15888, .T. ) ;
#9791 = DIRECTION ( 'NONE',  ( -1.000000000000000000, 0.000000000000000000, 0.000000000000000000 ) ) ;
#9792 = DIRECTION ( 'NONE',  ( 1.000000000000000000, 0.000000000000000000, 0.000000000000000000 ) ) ;
#9793 = ORIENTED_EDGE ( 'NONE', *, *, #4684, .T. ) ;
#9794 = CARTESIAN_POINT ( 'NONE',  ( -71.24615306438110451, 3.717815454563776711, 15.00000000000006928 ) ) ;
#9795 = CARTESIAN_POINT ( 'NONE',  ( -71.24615306438086293, 91.68240965456375591, -167.1454815528550739 ) ) ;
#9796 = CARTESIAN_POINT ( 'NONE',  ( -42.13624723507101066, 48.33286343412846975, 28.43491036791323623 ) ) ;
#9797 = CARTESIAN_POINT ( 'NONE',  ( -68.99615306438067819, 145.9084177316626949, -167.1454815528550739 ) ) ;
#9798 = ORIENTED_EDGE ( 'NONE', *, *, #6196, .T. ) ;
#9799 = EDGE_CURVE ( 'NONE', #3553, #16487, #16847, .T. ) ;
#9800 = CARTESIAN_POINT ( 'NONE',  ( -65.50906076758114693, 77.46608744949911340, -15.00000000000001421 ) ) ;
#9801 = LINE ( 'NONE', #7607, #1084 ) ;
#9802 = CARTESIAN_POINT ( 'NONE',  ( -74.59024599270496481, 107.8080920662734314, 23.45507754830875413 ) ) ;
#9803 = APPLICATION_CONTEXT ( 'automotive_design' ) ;
#9804 = CARTESIAN_POINT ( 'NONE',  ( 3.412248078327399625, -3.148451073394814337, -51.39674937110251562 ) ) ;
#9805 = CARTESIAN_POINT ( 'NONE',  ( -68.99615306438106188, 26.52789703166272517, -15.00000000000001421 ) ) ;
#9806 = VERTEX_POINT ( 'NONE', #11421 ) ;
#9807 = CARTESIAN_POINT ( 'NONE',  ( 95.45835937779683888, -32.62665103886256190, 3.000000000000000000 ) ) ;
#9808 = LINE ( 'NONE', #17001, #17337 ) ;
#9809 = LINE ( 'NONE', #8511, #15849 ) ;
#9810 = DIRECTION ( 'NONE',  ( 0.000000000000000000, 0.000000000000000000, 1.000000000000000000 ) ) ;
#9811 = ORIENTED_EDGE ( 'NONE', *, *, #14757, .T. ) ;
#9812 = VERTEX_POINT ( 'NONE', #17017 ) ;
#9813 = DIRECTION ( 'NONE',  ( 0.000000000000000000, 0.000000000000000000, 1.000000000000000000 ) ) ;
#9814 = ORIENTED_EDGE ( 'NONE', *, *, #4577, .T. ) ;
#9815 = CARTESIAN_POINT ( 'NONE',  ( -107.5926225674731853, 110.5691553257988460, -22.35917033480641791 ) ) ;
#9816 = DIRECTION ( 'NONE',  ( -1.000000000000000000, -0.000000000000000000, -0.000000000000000000 ) ) ;
#9817 = AXIS2_PLACEMENT_3D ( 'NONE', #5170, #11273, #18178 ) ;
#9818 = CARTESIAN_POINT ( 'NONE',  ( -65.06546592763085357, -95.65021616327642562, -45.05044770573176294 ) ) ;
#9819 = ORIENTED_EDGE ( 'NONE', *, *, #1982, .F. ) ;
#9820 = EDGE_CURVE ( 'NONE', #1460, #13724, #4303, .T. ) ;
#9821 = CARTESIAN_POINT ( 'NONE',  ( 0.5805565836007609004, 3.752776749732559924, -6.500000000000061284 ) ) ;
#9822 = DIRECTION ( 'NONE',  ( -1.000000000000000000, -0.000000000000000000, -0.000000000000000000 ) ) ;
#9823 = DIRECTION ( 'NONE',  ( -1.000000000000000000, 0.000000000000000000, 0.000000000000000000 ) ) ;
#9824 = CARTESIAN_POINT ( 'NONE',  ( 105.4583593777967963, -32.62665103886256190, 7.000000000000010658 ) ) ;
#9825 = VERTEX_POINT ( 'NONE', #11520 ) ;
#9826 = DIRECTION ( 'NONE',  ( 0.000000000000000000, 0.000000000000000000, 1.000000000000000000 ) ) ;
#9827 = VERTEX_POINT ( 'NONE', #10020 ) ;
#9828 = ADVANCED_FACE ( 'NONE', ( #15885 ), #14237, .T. ) ;
#9829 = CARTESIAN_POINT ( 'NONE',  ( 4.699999999999995737, 6.499999999999901412, 2.428612866367529932E-14 ) ) ;
#9830 = DIRECTION ( 'NONE',  ( 0.000000000000000000, 0.000000000000000000, 1.000000000000000000 ) ) ;
#9831 = ORIENTED_EDGE ( 'NONE', *, *, #9750, .F. ) ;
#9832 = CIRCLE ( 'NONE', #15503, 4.600000000000006750 ) ;
#9833 = ORIENTED_EDGE ( 'NONE', *, *, #18165, .F. ) ;
#9834 = EDGE_LOOP ( 'NONE', ( #2700, #13886, #9142, #5728 ) ) ;
#9835 = EDGE_CURVE ( 'NONE', #18083, #11856, #6628, .T. ) ;
#9836 = DIRECTION ( 'NONE',  ( 0.000000000000000000, 0.000000000000000000, -1.000000000000000000 ) ) ;
#9837 = DIRECTION ( 'NONE',  ( 0.9396926207859171987, 0.3420201433256444545, -1.086737899652999999E-16 ) ) ;
#9838 = EDGE_CURVE ( 'NONE', #10339, #2433, #13798, .T. ) ;
#9839 = DIRECTION ( 'NONE',  ( 1.000000000000000000, 0.000000000000000000, 0.000000000000000000 ) ) ;
#9840 = ADVANCED_FACE ( 'NONE', ( #13272 ), #5284, .T. ) ;
#9841 = CARTESIAN_POINT ( 'NONE',  ( -68.99615306438100504, 42.23586028166270978, -167.1454815528550739 ) ) ;
#9842 = CARTESIAN_POINT ( 'NONE',  ( 0.2578475836320997527, 4.367703157927319779, -5.434916218090905637 ) ) ;
#9843 = VERTEX_POINT ( 'NONE', #12413 ) ;
#9844 = CIRCLE ( 'NONE', #14324, 10.65431531532567888 ) ;
#9845 = DIRECTION ( 'NONE',  ( -1.000000000000000000, 4.062187864517842136E-15, 1.692578276882434470E-16 ) ) ;
#9846 = ORIENTED_EDGE ( 'NONE', *, *, #15795, .T. ) ;
#9847 = DIRECTION ( 'NONE',  ( 0.000000000000000000, -0.000000000000000000, 1.000000000000000000 ) ) ;
#9848 = DIRECTION ( 'NONE',  ( 0.000000000000000000, 1.000000000000000000, 0.000000000000000000 ) ) ;
#9849 = ORIENTED_EDGE ( 'NONE', *, *, #13282, .T. ) ;
#9850 = ADVANCED_FACE ( 'NONE', ( #10452 ), #13447, .T. ) ;
#9851 = EDGE_CURVE ( 'NONE', #13685, #9953, #10824, .T. ) ;
#9852 = EDGE_CURVE ( 'NONE', #6748, #9223, #18001, .T. ) ;
#9853 = CARTESIAN_POINT ( 'NONE',  ( -68.99615306438093398, 49.13390143813026611, 15.00000000000006928 ) ) ;
#9854 = VERTEX_POINT ( 'NONE', #16598 ) ;
#9855 = EDGE_CURVE ( 'NONE', #16487, #11023, #13806, .T. ) ;
#9856 = AXIS2_PLACEMENT_3D ( 'NONE', #7348, #2866, #15939 ) ;
#9857 = ORIENTED_EDGE ( 'NONE', *, *, #2571, .T. ) ;
#9858 = EDGE_CURVE ( 'NONE', #3659, #14934, #3786, .T. ) ;
#9859 = VECTOR ( 'NONE', #5926, 1000.000000000000000 ) ;
#9860 = CARTESIAN_POINT ( 'NONE',  ( -57.08002265617300708, 84.22855780814606419, -62.50000000000000000 ) ) ;
#9861 = DIRECTION ( 'NONE',  ( 1.000000000000000000, 0.000000000000000000, 0.000000000000000000 ) ) ;
#9862 = DIRECTION ( 'NONE',  ( 1.000000000000000000, 0.000000000000000000, 0.000000000000000000 ) ) ;
#9863 = ORIENTED_EDGE ( 'NONE', *, *, #18187, .T. ) ;
#9864 = ORIENTED_EDGE ( 'NONE', *, *, #7014, .F. ) ;
#9865 = EDGE_CURVE ( 'NONE', #1935, #3596, #6046, .T. ) ;
#9866 = CARTESIAN_POINT ( 'NONE',  ( 15.23320273812466041, -19.34983604512934363, -54.79921157549233612 ) ) ;
#9867 = EDGE_CURVE ( 'NONE', #2737, #15821, #14662, .T. ) ;
#9868 = CARTESIAN_POINT ( 'NONE',  ( -68.99615306438067819, 143.3816809381303585, 15.00000000000006928 ) ) ;
#9869 = ORIENTED_EDGE ( 'NONE', *, *, #8066, .F. ) ;
#9870 = CARTESIAN_POINT ( 'NONE',  ( -107.5926225674731711, 54.12595869546677818, 25.00000000000000000 ) ) ;
#9871 = DIRECTION ( 'NONE',  ( -5.204170427930409450E-16, 0.000000000000000000, 1.000000000000000000 ) ) ;
#9872 = CARTESIAN_POINT ( 'NONE',  ( -92.59262256747318531, -1.909541702982995504E-14, 0.000000000000000000 ) ) ;
#9873 = EDGE_LOOP ( 'NONE', ( #7516, #16278, #12206, #10320, #2865, #14788, #6541 ) ) ;
#9874 = DIRECTION ( 'NONE',  ( -0.9396926207859158664, 0.3420201433256481738, 1.086737899652998397E-16 ) ) ;
#9875 = DIRECTION ( 'NONE',  ( -1.000000000000000000, -0.000000000000000000, -0.000000000000000000 ) ) ;
#9876 = ORIENTED_EDGE ( 'NONE', *, *, #5526, .T. ) ;
#9877 = EDGE_CURVE ( 'NONE', #748, #2148, #10510, .T. ) ;
#9878 = CIRCLE ( 'NONE', #9263, 170.8515291679562154 ) ;
#9879 = DIRECTION ( 'NONE',  ( 1.000000000000000000, 0.000000000000000000, 0.000000000000000000 ) ) ;
#9880 = ORIENTED_EDGE ( 'NONE', *, *, #2293, .T. ) ;
#9881 = VECTOR ( 'NONE', #17759, 1000.000000000000000 ) ;
#9882 = DIRECTION ( 'NONE',  ( 1.000000000000000000, 2.062304371594500494E-16, 0.000000000000000000 ) ) ;
#9883 = ORIENTED_EDGE ( 'NONE', *, *, #8937, .F. ) ;
#9884 = VECTOR ( 'NONE', #15510, 1000.000000000000000 ) ;
#9885 = VERTEX_POINT ( 'NONE', #453 ) ;
#9886 = AXIS2_PLACEMENT_3D ( 'NONE', #12055, #6228, #14759 ) ;
#9887 = DIRECTION ( 'NONE',  ( 1.156482317317869999E-16, 0.000000000000000000, 1.000000000000000000 ) ) ;
#9888 = VERTEX_POINT ( 'NONE', #16677 ) ;
#9889 = VECTOR ( 'NONE', #15605, 1000.000000000000227 ) ;
#9890 = DIRECTION ( 'NONE',  ( 0.000000000000000000, 0.000000000000000000, 1.000000000000000000 ) ) ;
#9891 = DIRECTION ( 'NONE',  ( 0.000000000000000000, -0.4999999999999999445, 0.8660254037844387076 ) ) ;
#9892 = VECTOR ( 'NONE', #16604, 1000.000000000000000 ) ;
#9893 = CARTESIAN_POINT ( 'NONE',  ( -9.128655484568604095, 23.76631003692282462, 41.91653839390071568 ) ) ;
#9894 = DIRECTION ( 'NONE',  ( 0.000000000000000000, 0.000000000000000000, 1.000000000000000000 ) ) ;
#9895 = ORIENTED_EDGE ( 'NONE', *, *, #16947, .T. ) ;
#9896 = LINE ( 'NONE', #2689, #9889 ) ;
#9897 = CARTESIAN_POINT ( 'NONE',  ( 98.04320049944426785, 73.84851424090838634, 62.50000000000001421 ) ) ;
#9898 = CARTESIAN_POINT ( 'NONE',  ( -71.24615306438067819, 144.2006139652292518, -167.1454815528550739 ) ) ;
#9899 = CARTESIAN_POINT ( 'NONE',  ( -68.99615306438100504, 49.13390143813029454, -167.1454815528550739 ) ) ;
#9900 = ORIENTED_EDGE ( 'NONE', *, *, #10884, .F. ) ;
#9901 = AXIS2_PLACEMENT_3D ( 'NONE', #221, #7247, #17324 ) ;
#9902 = PLANE ( 'NONE',  #8539 ) ;
#9903 = CARTESIAN_POINT ( 'NONE',  ( -67.44681693414594292, 91.21279551874751235, 15.00000000000006928 ) ) ;
#9904 = DIRECTION ( 'NONE',  ( -1.000000000000000000, 0.000000000000000000, 0.000000000000000000 ) ) ;
#9905 = AXIS2_PLACEMENT_3D ( 'NONE', #2368, #13902, #6784 ) ;
#9906 = CIRCLE ( 'NONE', #2425, 3.445500000000021767 ) ;
#9907 = LINE ( 'NONE', #2802, #5075 ) ;
#9908 = ORIENTED_EDGE ( 'NONE', *, *, #11457, .F. ) ;
#9909 = ORIENTED_EDGE ( 'NONE', *, *, #15769, .T. ) ;
#9910 = CARTESIAN_POINT ( 'NONE',  ( -68.99615306438067819, 145.9084177316626949, 15.00000000000006928 ) ) ;
#9911 = ADVANCED_FACE ( 'NONE', ( #9062 ), #7558, .F. ) ;
#9912 = AXIS2_PLACEMENT_3D ( 'NONE', #8993, #14864, #16276 ) ;
#9913 = ORIENTED_EDGE ( 'NONE', *, *, #14054, .F. ) ;
#9914 = CARTESIAN_POINT ( 'NONE',  ( -71.24615306438086293, 91.68240965456375591, -15.00000000000001421 ) ) ;
#9915 = CARTESIAN_POINT ( 'NONE',  ( -68.99615306438066398, 127.6737176881302673, 15.00000000000006928 ) ) ;
#9916 = CARTESIAN_POINT ( 'NONE',  ( 0.000000000000000000, 0.000000000000000000, 0.000000000000000000 ) ) ;
#9917 = ORIENTED_EDGE ( 'NONE', *, *, #1830, .F. ) ;
#9918 = CARTESIAN_POINT ( 'NONE',  ( -66.16666462472026922, 110.5025503192935474, -27.99999999999999289 ) ) ;
#9919 = CIRCLE ( 'NONE', #4811, 4.599999999999992539 ) ;
#9920 = VECTOR ( 'NONE', #17135, 1000.000000000000000 ) ;
#9921 = CARTESIAN_POINT ( 'NONE',  ( -71.24615306438091977, 72.83285375456371469, -167.1454815528550739 ) ) ;
#9922 = PLANE ( 'NONE',  #5546 ) ;
#9923 = DIRECTION ( 'NONE',  ( 0.000000000000000000, 1.000000000000000000, -1.224646799147353207E-16 ) ) ;
#9924 = ORIENTED_EDGE ( 'NONE', *, *, #13046, .F. ) ;
#9925 = CARTESIAN_POINT ( 'NONE',  ( -71.24615306438103346, 44.55851990456372391, -167.1454815528550739 ) ) ;
#9926 = ORIENTED_EDGE ( 'NONE', *, *, #7000, .F. ) ;
#9927 = AXIS2_PLACEMENT_3D ( 'NONE', #6199, #13619, #11926 ) ;
#9928 = PLANE ( 'NONE',  #2718 ) ;
#9929 = CARTESIAN_POINT ( 'NONE',  ( -65.06546592763099568, -91.08423613455721579, -28.18308811886532084 ) ) ;
#9930 = ORIENTED_EDGE ( 'NONE', *, *, #17937, .T. ) ;
#9931 = VERTEX_POINT ( 'NONE', #11773 ) ;
#9932 = AXIS2_PLACEMENT_3D ( 'NONE', #10624, #13339, #4806 ) ;
#9933 = EDGE_LOOP ( 'NONE', ( #15707, #11724, #11743, #6662 ) ) ;
#9934 = CARTESIAN_POINT ( 'NONE',  ( -45.39578445746348478, 88.67024416760654049, -15.00000000000001421 ) ) ;
#9935 = CARTESIAN_POINT ( 'NONE',  ( -92.59262256747318531, 0.3328663868096687350, -25.00000000000000000 ) ) ;
#9936 = CARTESIAN_POINT ( 'NONE',  ( -71.24615306438093398, 53.98329785456376584, 15.00000000000006928 ) ) ;
#9937 = CIRCLE ( 'NONE', #10236, 4.000000000000003553 ) ;
#9938 = ADVANCED_FACE ( 'NONE', ( #4732 ), #14750, .T. ) ;
#9939 = FACE_OUTER_BOUND ( 'NONE', #1248, .T. ) ;
#9940 = CARTESIAN_POINT ( 'NONE',  ( -48.21445538031289857, 89.37090336996882911, 15.00000000000006928 ) ) ;
#9941 = ORIENTED_EDGE ( 'NONE', *, *, #13067, .F. ) ;
#9942 = LINE ( 'NONE', #15654, #3039 ) ;
#9943 = ORIENTED_EDGE ( 'NONE', *, *, #13854, .F. ) ;
#9944 = PLANE ( 'NONE',  #11162 ) ;
#9945 = CIRCLE ( 'NONE', #5139, 10.24900000000001477 ) ;
#9946 = VECTOR ( 'NONE', #17419, 1000.000000000000000 ) ;
#9947 = CARTESIAN_POINT ( 'NONE',  ( -57.08002265617300708, 84.22855780814606419, 15.00000000000006928 ) ) ;
#9948 = VERTEX_POINT ( 'NONE', #10369 ) ;
#9949 = CARTESIAN_POINT ( 'NONE',  ( -110.3711597500467860, -91.10977358899565104, -10.13292356933350113 ) ) ;
#9950 = ORIENTED_EDGE ( 'NONE', *, *, #14954, .F. ) ;
#9951 = EDGE_CURVE ( 'NONE', #663, #8598, #1949, .T. ) ;
#9952 = VECTOR ( 'NONE', #4509, 1000.000000000000000 ) ;
#9953 = VERTEX_POINT ( 'NONE', #532 ) ;
#9954 = VECTOR ( 'NONE', #4848, 1000.000000000000000 ) ;
#9955 = CIRCLE ( 'NONE', #4550, 3.999999999999989786 ) ;
#9956 =( LENGTH_UNIT ( ) NAMED_UNIT ( * ) SI_UNIT ( .MILLI., .METRE. ) );
#9957 = FACE_OUTER_BOUND ( 'NONE', #1050, .T. ) ;
#9958 = DIRECTION ( 'NONE',  ( 0.000000000000000000, 1.000000000000000000, 0.000000000000000000 ) ) ;
#9959 = EDGE_CURVE ( 'NONE', #11836, #7586, #10226, .T. ) ;
#9960 = ORIENTED_EDGE ( 'NONE', *, *, #13618, .T. ) ;
#9961 = ADVANCED_FACE ( 'NONE', ( #16247 ), #14840, .T. ) ;
#9962 = VERTEX_POINT ( 'NONE', #5745 ) ;
#9963 = CARTESIAN_POINT ( 'NONE',  ( -71.24615306438094819, 68.80239036522922902, 15.00000000000006928 ) ) ;
#9964 = FACE_OUTER_BOUND ( 'NONE', #10118, .T. ) ;
#9965 = EDGE_LOOP ( 'NONE', ( #1336, #13361 ) ) ;
#9966 = VECTOR ( 'NONE', #8003, 1000.000000000000000 ) ;
#9967 = CARTESIAN_POINT ( 'NONE',  ( -71.24615306438109030, 27.96168591522921076, 15.00000000000006928 ) ) ;
#9968 = CARTESIAN_POINT ( 'NONE',  ( -57.08002265617300708, 84.22855780814606419, -15.00000000000001421 ) ) ;
#9969 = DIRECTION ( 'NONE',  ( 0.000000000000000000, 0.000000000000000000, -1.000000000000000000 ) ) ;
#9970 = VERTEX_POINT ( 'NONE', #1177 ) ;
#9971 = DIRECTION ( 'NONE',  ( -0.9396926207859097602, 0.3420201433256649381, -4.890320548438455808E-16 ) ) ;
#9972 = ORIENTED_EDGE ( 'NONE', *, *, #6143, .F. ) ;
#9973 = ADVANCED_FACE ( 'NONE', ( #8568 ), #14085, .T. ) ;
#9974 = CIRCLE ( 'NONE', #9655, 45.40389983439752086 ) ;
#9976 = ORIENTED_EDGE ( 'NONE', *, *, #9291, .F. ) ;
#9975 = AXIS2_PLACEMENT_3D ( 'NONE', #15970, #17539, #3239 ) ;
#9977 = EDGE_CURVE ( 'NONE', #1662, #7503, #5652, .T. ) ;
#9978 = CARTESIAN_POINT ( 'NONE',  ( -66.71217848887407342, 56.48326379586188750, -24.23239327750837191 ) ) ;
#9979 = ORIENTED_EDGE ( 'NONE', *, *, #7113, .T. ) ;
#9980 = ADVANCED_FACE ( 'NONE', ( #10058 ), #2864, .T. ) ;
#9981 = EDGE_CURVE ( 'NONE', #2087, #3821, #9955, .T. ) ;
#9982 = EDGE_LOOP ( 'NONE', ( #6792, #14238, #17918, #50 ) ) ;
#9983 = LINE ( 'NONE', #2680, #14172 ) ;
#9984 = DIRECTION ( 'NONE',  ( 0.000000000000000000, 5.551115123125748189E-17, 1.000000000000000000 ) ) ;
#9985 = ADVANCED_FACE ( 'NONE', ( #5563 ), #1268, .T. ) ;
#9986 = ORIENTED_EDGE ( 'NONE', *, *, #13675, .F. ) ;
#9987 = PRODUCT_DEFINITION_FORMATION_WITH_SPECIFIED_SOURCE ( 'ANY', '', #17885, .NOT_KNOWN. ) ;
#9988 = VECTOR ( 'NONE', #15696, 1000.000000000000000 ) ;
#9989 = FACE_OUTER_BOUND ( 'NONE', #3672, .T. ) ;
#9991 = VECTOR ( 'NONE', #9674, 1000.000000000000000 ) ;
#9990 = DIRECTION ( 'NONE',  ( 0.3420201433256481738, -0.9396926207859158664, 0.000000000000000000 ) ) ;
#9992 = CARTESIAN_POINT ( 'NONE',  ( -12.80512717543878942, 28.43086510689403568, 39.77885264312817526 ) ) ;
#9993 = PLANE ( 'NONE',  #1617 ) ;
#9994 = ORIENTED_EDGE ( 'NONE', *, *, #11467, .T. ) ;
#9995 = DIRECTION ( 'NONE',  ( -0.000000000000000000, -0.000000000000000000, 1.000000000000000000 ) ) ;
#9996 = DIRECTION ( 'NONE',  ( 2.750867011994134873E-15, 0.000000000000000000, 1.000000000000000000 ) ) ;
#9997 = DIRECTION ( 'NONE',  ( 0.9396926207859110924, 0.3420201433256612189, -1.086737899652992973E-16 ) ) ;
#9998 = ORIENTED_EDGE ( 'NONE', *, *, #11126, .T. ) ;
#9999 = CONICAL_SURFACE ( 'NONE', #4003, 3.999999999999989786, 1.029744258676652091 ) ;
#10000 = CARTESIAN_POINT ( 'NONE',  ( -68.99615306438097662, 61.08541618166268705, -167.1454815528550739 ) ) ;
#10001 = DIRECTION ( 'NONE',  ( 0.000000000000000000, 0.000000000000000000, 1.000000000000000000 ) ) ;
#10002 = DIRECTION ( 'NONE',  ( -0.000000000000000000, -0.000000000000000000, -1.000000000000000000 ) ) ;
#10003 = CARTESIAN_POINT ( 'NONE',  ( -68.99615306438070661, 137.0984956381303164, -15.00000000000001421 ) ) ;
#10004 = ORIENTED_EDGE ( 'NONE', *, *, #8733, .T. ) ;
#10005 = AXIS2_PLACEMENT_3D ( 'NONE', #17869, #3476, #16287 ) ;
#10006 = ADVANCED_FACE ( 'NONE', ( #15483 ), #15395, .F. ) ;
#10007 = EDGE_LOOP ( 'NONE', ( #9433, #1858, #2429, #1368, #10464, #5099 ) ) ;
#10008 = FACE_OUTER_BOUND ( 'NONE', #5288, .T. ) ;
#10009 = VECTOR ( 'NONE', #3043, 1000.000000000000000 ) ;
#10010 = EDGE_LOOP ( 'NONE', ( #13259, #2499, #4036, #10375 ) ) ;
#10011 = CARTESIAN_POINT ( 'NONE',  ( -67.36180031798897971, 111.7399260588586287, -22.93227665730716325 ) ) ;
#10012 = SHAPE_REPRESENTATION_RELATIONSHIP ( 'NONE' , 'NONE' ,  #17553, #7459 ) ;
#10013 = CARTESIAN_POINT ( 'NONE',  ( -68.99615306438103346, 32.81108233166271759, 15.00000000000006928 ) ) ;
#10014 = ORIENTED_EDGE ( 'NONE', *, *, #2516, .T. ) ;
#10015 = VECTOR ( 'NONE', #10629, 1000.000000000000000 ) ;
#10016 = CARTESIAN_POINT ( 'NONE',  ( 0.000000000000000000, -2.914335439641035919E-13, -6.500000000000019540 ) ) ;
#10017 = CIRCLE ( 'NONE', #9095, 4.599999999999999645 ) ;
#10018 = DIRECTION ( 'NONE',  ( 0.000000000000000000, 0.000000000000000000, 1.000000000000000000 ) ) ;
#10019 =( NAMED_UNIT ( * ) PLANE_ANGLE_UNIT ( ) SI_UNIT ( $, .RADIAN. ) );
#10020 = CARTESIAN_POINT ( 'NONE',  ( -71.24615306438079188, 112.7846874652292399, -15.00000000000001421 ) ) ;
#10021 = ORIENTED_EDGE ( 'NONE', *, *, #10334, .F. ) ;
#10022 = CARTESIAN_POINT ( 'NONE',  ( -68.99615306438091977, 73.65178678166269322, -167.1454815528550739 ) ) ;
#10023 = LINE ( 'NONE', #15731, #8074 ) ;
#10024 = VERTEX_POINT ( 'NONE', #43 ) ;
#10025 = CARTESIAN_POINT ( 'NONE',  ( -71.24615306438086293, 90.79353891522923448, -15.00000000000001421 ) ) ;
#10026 = LINE ( 'NONE', #1333, #5329 ) ;
#10027 = ORIENTED_EDGE ( 'NONE', *, *, #14855, .F. ) ;
#10028 = ORIENTED_EDGE ( 'NONE', *, *, #699, .T. ) ;
#10029 = VECTOR ( 'NONE', #483, 1000.000000000000000 ) ;
#10030 = CIRCLE ( 'NONE', #3414, 20.99999999999999645 ) ;
#10031 = DIRECTION ( 'NONE',  ( 0.000000000000000000, 0.4999999999999999445, -0.8660254037844387076 ) ) ;
#10032 = DIRECTION ( 'NONE',  ( 1.000000000000000000, 0.000000000000000000, 0.000000000000000000 ) ) ;
#10033 = DIRECTION ( 'NONE',  ( 0.000000000000000000, 0.000000000000000000, 1.000000000000000000 ) ) ;
#10034 = CARTESIAN_POINT ( 'NONE',  ( -71.24615306438080609, 109.6430948152292189, -167.1454815528550739 ) ) ;
#10035 = FACE_OUTER_BOUND ( 'NONE', #12679, .T. ) ;
#10036 = ORIENTED_EDGE ( 'NONE', *, *, #13051, .F. ) ;
#10037 = EDGE_CURVE ( 'NONE', #15366, #14959, #2477, .T. ) ;
#10038 = DIRECTION ( 'NONE',  ( -5.204170427930409450E-16, 0.000000000000000000, 1.000000000000000000 ) ) ;
#10039 = ORIENTED_EDGE ( 'NONE', *, *, #16467, .F. ) ;
#10040 = CARTESIAN_POINT ( 'NONE',  ( -68.12361985383350316, 84.22855780814606419, -28.00000000000000355 ) ) ;
#10041 = AXIS2_PLACEMENT_3D ( 'NONE', #15213, #2396, #5210 ) ;
#10042 = VECTOR ( 'NONE', #14704, 1000.000000000000000 ) ;
#10043 = CARTESIAN_POINT ( 'NONE',  ( -67.59262256747315689, 50.58224449241410525, 15.00000000000006750 ) ) ;
#10044 = ORIENTED_EDGE ( 'NONE', *, *, #8599, .F. ) ;
#10045 = DIRECTION ( 'NONE',  ( 0.000000000000000000, 0.000000000000000000, 1.000000000000000000 ) ) ;
#10046 = ORIENTED_EDGE ( 'NONE', *, *, #17180, .T. ) ;
#10047 = ORIENTED_EDGE ( 'NONE', *, *, #4576, .F. ) ;
#10048 = DIRECTION ( 'NONE',  ( -1.000000000000000000, -0.000000000000000000, -0.000000000000000000 ) ) ;
#10049 = PLANE ( 'NONE',  #6378 ) ;
#10050 = DIRECTION ( 'NONE',  ( 0.000000000000000000, 1.000000000000000000, 0.000000000000000000 ) ) ;
#10051 = ORIENTED_EDGE ( 'NONE', *, *, #16225, .F. ) ;
#10052 = CONTEXT_DEPENDENT_SHAPE_REPRESENTATION ( #10389, #17737 ) ;
#10053 = CARTESIAN_POINT ( 'NONE',  ( -26.13860949178274851, -94.06000665574431707, 6.066633903742967071 ) ) ;
#10054 = CARTESIAN_POINT ( 'NONE',  ( -68.76426085488260753, 88.67024416760638417, -167.1454815528550739 ) ) ;
#10055 = ORIENTED_EDGE ( 'NONE', *, *, #2250, .T. ) ;
#10056 = FACE_OUTER_BOUND ( 'NONE', #15029, .T. ) ;
#10057 = DIRECTION ( 'NONE',  ( -0.000000000000000000, -0.000000000000000000, -1.000000000000000000 ) ) ;
#10058 = FACE_OUTER_BOUND ( 'NONE', #11422, .T. ) ;
#10059 = VERTEX_POINT ( 'NONE', #14182 ) ;
#10060 = CARTESIAN_POINT ( 'NONE',  ( -36.03642545851251100, 84.22855780814606419, 77.50000000000000000 ) ) ;
#10061 = EDGE_LOOP ( 'NONE', ( #6316, #13462, #11586, #11189 ) ) ;
#10062 = ORIENTED_EDGE ( 'NONE', *, *, #10065, .F. ) ;
#10063 = EDGE_CURVE ( 'NONE', #16572, #2924, #5453, .T. ) ;
#10064 = CARTESIAN_POINT ( 'NONE',  ( -127.5926225674731995, 110.5691553257988460, 30.35917033480641081 ) ) ;
#10065 = EDGE_CURVE ( 'NONE', #1178, #7613, #1371, .T. ) ;
#10066 = ORIENTED_EDGE ( 'NONE', *, *, #3641, .T. ) ;
#10067 = CARTESIAN_POINT ( 'NONE',  ( -71.24615306438074924, 132.5231141045637457, -15.00000000000001421 ) ) ;
#10068 = PLANE ( 'NONE',  #3698 ) ;
#10069 = DIRECTION ( 'NONE',  ( 0.000000000000000000, 1.000000000000000000, 0.000000000000000000 ) ) ;
#10070 = ORIENTED_EDGE ( 'NONE', *, *, #7794, .F. ) ;
#10071 = EDGE_CURVE ( 'NONE', #10167, #11961, #4259, .T. ) ;
#10072 = PLANE ( 'NONE',  #5949 ) ;
#10073 = DIRECTION ( 'NONE',  ( 0.000000000000000000, 0.000000000000000000, -1.000000000000000000 ) ) ;
#10074 = DIRECTION ( 'NONE',  ( 0.000000000000000000, 0.000000000000000000, 1.000000000000000000 ) ) ;
#10075 = EDGE_CURVE ( 'NONE', #13404, #10351, #18481, .T. ) ;
#10076 = CARTESIAN_POINT ( 'NONE',  ( -54.80923614058017534, 94.79374675277698259, -15.00000000000001421 ) ) ;
#10077 = ORIENTED_EDGE ( 'NONE', *, *, #12838, .T. ) ;
#10078 = EDGE_CURVE ( 'NONE', #14184, #115, #1094, .T. ) ;
#10079 = CARTESIAN_POINT ( 'NONE',  ( -71.24615306438109030, 25.70896400456376796, -167.1454815528550739 ) ) ;
#10080 = DIRECTION ( 'NONE',  ( 0.000000000000000000, -5.551115123125748189E-17, -1.000000000000000000 ) ) ;
#10081 = DIRECTION ( 'NONE',  ( -0.3197242186372270534, 0.9475106458593564041, 0.000000000000000000 ) ) ;
#10082 = EDGE_LOOP ( 'NONE', ( #11093, #18038, #3971, #9631 ) ) ;
#10083 = CARTESIAN_POINT ( 'NONE',  ( 15.23320273812467462, -111.0842361345572158, -3.000000000000000000 ) ) ;
#10084 = ADVANCED_FACE ( 'NONE', ( #18196 ), #3662, .T. ) ;
#10085 = EDGE_CURVE ( 'NONE', #13750, #15130, #5157, .T. ) ;
#10086 = DIRECTION ( 'NONE',  ( 0.000000000000000000, 0.000000000000000000, 1.000000000000000000 ) ) ;
#10087 = EDGE_CURVE ( 'NONE', #10621, #14872, #16883, .T. ) ;
#10088 = CARTESIAN_POINT ( 'NONE',  ( -68.99615306438106188, 24.00116023813026445, -167.1454815528550739 ) ) ;
#10089 = ORIENTED_EDGE ( 'NONE', *, *, #1982, .T. ) ;
#10090 = ORIENTED_EDGE ( 'NONE', *, *, #7684, .T. ) ;
#10091 = ADVANCED_FACE ( 'NONE', ( #8375 ), #6972, .T. ) ;
#10092 = LINE ( 'NONE', #11668, #12671 ) ;
#10093 = DIRECTION ( 'NONE',  ( 1.000000000000000000, 0.000000000000000000, 0.000000000000000000 ) ) ;
#10094 = CARTESIAN_POINT ( 'NONE',  ( -92.59262256747321373, 117.8748711238780373, -15.00000000000000711 ) ) ;
#10095 = CARTESIAN_POINT ( 'NONE',  ( -64.09025127992788384, 50.58224449241410525, 35.00000000000000000 ) ) ;
#10096 = CARTESIAN_POINT ( 'NONE',  ( -60.71745612804021874, -91.12516132330414109, -39.81918451580444440 ) ) ;
#10097 = EDGE_LOOP ( 'NONE', ( #1997, #15663, #18369, #6018 ) ) ;
#10098 = DIRECTION ( 'NONE',  ( -0.9475106458593564041, 0.3197242186372270534, 0.000000000000000000 ) ) ;
#10099 = DIRECTION ( 'NONE',  ( -1.000000000000000000, 0.000000000000000000, 0.000000000000000000 ) ) ;
#10100 = EDGE_CURVE ( 'NONE', #3118, #17521, #6179, .T. ) ;
#10101 = CARTESIAN_POINT ( 'NONE',  ( -40.53769224766538315, 54.09612659366786147, 24.44902958348917466 ) ) ;
#10102 = CARTESIAN_POINT ( 'NONE',  ( 0.05613245601034763665, 1.278525034529172544, 6.499999999999984013 ) ) ;
#10103 = ORIENTED_EDGE ( 'NONE', *, *, #14221, .F. ) ;
#10104 = EDGE_CURVE ( 'NONE', #6695, #15813, #11728, .T. ) ;
#10105 = CARTESIAN_POINT ( 'NONE',  ( -36.62600694138065904, 89.18782894963364072, 68.14764070353975001 ) ) ;
#10106 = CARTESIAN_POINT ( 'NONE',  ( -68.99615306438094819, 54.80223088166269463, -167.1454815528550739 ) ) ;
#10107 = EDGE_LOOP ( 'NONE', ( #1977, #2196, #10286, #1372, #7919, #18093, #4791, #8913, #12158, #16065 ) ) ;
#10108 = DIRECTION ( 'NONE',  ( 0.000000000000000000, 0.000000000000000000, -1.000000000000000000 ) ) ;
#10109 = CARTESIAN_POINT ( 'NONE',  ( -71.24615306438086293, 87.65194626522927024, -167.1454815528550739 ) ) ;
#10110 = ORIENTED_EDGE ( 'NONE', *, *, #16258, .F. ) ;
#10111 = ORIENTED_EDGE ( 'NONE', *, *, #13726, .T. ) ;
#10112 = VECTOR ( 'NONE', #7008, 1000.000000000000000 ) ;
#10113 = CARTESIAN_POINT ( 'NONE',  ( -68.99615306438096241, 61.70027203813027938, -15.00000000000001421 ) ) ;
#10114 = CARTESIAN_POINT ( 'NONE',  ( -71.24615306438086293, 101.1071876045637055, -167.1454815528550739 ) ) ;
#10115 = DIRECTION ( 'NONE',  ( 4.675871521838984962E-16, -1.000000000000000000, 0.000000000000000000 ) ) ;
#10116 = LINE ( 'NONE', #10205, #14916 ) ;
#10117 = DIRECTION ( 'NONE',  ( 0.000000000000000000, 1.000000000000000000, 0.000000000000000000 ) ) ;
#10118 = EDGE_LOOP ( 'NONE', ( #7573, #11603, #14732, #4160 ) ) ;
#10119 = DIRECTION ( 'NONE',  ( 0.000000000000000000, 0.5000000000000008882, -0.8660254037844381525 ) ) ;
#10120 = ORIENTED_EDGE ( 'NONE', *, *, #10626, .T. ) ;
#10121 = LINE ( 'NONE', #16079, #15018 ) ;
#10122 = DIRECTION ( 'NONE',  ( -5.204170427930409450E-16, 0.000000000000000000, 1.000000000000000000 ) ) ;
#10123 = CONICAL_SURFACE ( 'NONE', #4432, 3.999999999999982681, 1.029744258676651203 ) ;
#10124 = ORIENTED_EDGE ( 'NONE', *, *, #229, .T. ) ;
#10125 = CARTESIAN_POINT ( 'NONE',  ( -70.71978124295708312, -96.08423613455721579, 28.18308811886538479 ) ) ;
#10126 = VERTEX_POINT ( 'NONE', #13228 ) ;
#10127 = EDGE_CURVE ( 'NONE', #2450, #2040, #12948, .T. ) ;
#10128 = VERTEX_POINT ( 'NONE', #4426 ) ;
#10129 = DIRECTION ( 'NONE',  ( -5.204170427930409450E-16, 0.000000000000000000, 1.000000000000000000 ) ) ;
#10130 = AXIS2_PLACEMENT_3D ( 'NONE', #15156, #2340, #1341 ) ;
#10131 = LINE ( 'NONE', #217, #7888 ) ;
#10132 = CARTESIAN_POINT ( 'NONE',  ( -83.12361985383351737, 84.22855780814606419, 37.50000000000000000 ) ) ;
#10133 = ORIENTED_EDGE ( 'NONE', *, *, #12225, .T. ) ;
#10134 = CONTEXT_DEPENDENT_SHAPE_REPRESENTATION ( #5616, #12074 ) ;
#10135 = EDGE_CURVE ( 'NONE', #1935, #11356, #15637, .T. ) ;
#10136 = VERTEX_POINT ( 'NONE', #3290 ) ;
#10137 = FACE_OUTER_BOUND ( 'NONE', #9608, .T. ) ;
#10138 = DIRECTION ( 'NONE',  ( -0.000000000000000000, -0.000000000000000000, -1.000000000000000000 ) ) ;
#10139 = LINE ( 'NONE', #10410, #10838 ) ;
#10140 = ORIENTED_EDGE ( 'NONE', *, *, #10411, .F. ) ;
#10141 = DIRECTION ( 'NONE',  ( 0.000000000000000000, -5.551115123125747573E-17, -1.000000000000000000 ) ) ;
#10142 = ORIENTED_EDGE ( 'NONE', *, *, #4582, .T. ) ;
#10143 = ORIENTED_EDGE ( 'NONE', *, *, #14068, .T. ) ;
#10144 = VECTOR ( 'NONE', #8858, 1000.000000000000000 ) ;
#10145 = VECTOR ( 'NONE', #2108, 1000.000000000000000 ) ;
#10146 = ORIENTED_EDGE ( 'NONE', *, *, #137, .F. ) ;
#10147 = CARTESIAN_POINT ( 'NONE',  ( -68.99615306438091977, 73.65178678166269322, -15.00000000000001421 ) ) ;
#10148 = DIRECTION ( 'NONE',  ( 1.000000000000000000, 0.000000000000000000, 0.000000000000000000 ) ) ;
#10149 = VERTEX_POINT ( 'NONE', #9013 ) ;
#10150 = CARTESIAN_POINT ( 'NONE',  ( 124.5381772159375942, -46.83756720124470263, -57.00000000000000000 ) ) ;
#10151 = LINE ( 'NONE', #15859, #17898 ) ;
#10152 = CARTESIAN_POINT ( 'NONE',  ( -71.24615306438097662, 63.40807580456375803, -15.00000000000001421 ) ) ;
#10153 = CIRCLE ( 'NONE', #6254, 40.40389983439752086 ) ;
#10154 = DIRECTION ( 'NONE',  ( -0.9396926207859088720, 0.3420201433256675472, 1.086737899652990385E-16 ) ) ;
#10155 = EDGE_LOOP ( 'NONE', ( #5324, #2901, #18268, #17624 ) ) ;
#10156 = EDGE_CURVE ( 'NONE', #7359, #11134, #7249, .T. ) ;
#10157 = DIRECTION ( 'NONE',  ( 1.156482317317869999E-16, 0.000000000000000000, 1.000000000000000000 ) ) ;
#10158 = AXIS2_PLACEMENT_3D ( 'NONE', #2879, #7964, #12094 ) ;
#10159 = PLANE ( 'NONE',  #18299 ) ;
#10160 = CARTESIAN_POINT ( 'NONE',  ( -102.5926225674731569, 65.58224449241410525, -20.00000000000000355 ) ) ;
#10161 = VERTEX_POINT ( 'NONE', #142 ) ;
#10162 = CARTESIAN_POINT ( 'NONE',  ( -71.24615306438114715, 9.112130015229229940, 15.00000000000006928 ) ) ;
#10163 = CARTESIAN_POINT ( 'NONE',  ( -112.5926225674731995, 50.58224449241410525, 35.00000000000000000 ) ) ;
#10164 = EDGE_LOOP ( 'NONE', ( #9880, #3154, #15011, #11695, #12319, #17745, #18451, #8088, #12298, #1504 ) ) ;
#10166 = EDGE_CURVE ( 'NONE', #10924, #3445, #10139, .T. ) ;
#10165 = AXIS2_PLACEMENT_3D ( 'NONE', #7737, #13451, #3080 ) ;
#10167 = VERTEX_POINT ( 'NONE', #12972 ) ;
#10168 = EDGE_CURVE ( 'NONE', #5660, #6083, #3130, .T. ) ;
#10169 = CIRCLE ( 'NONE', #6569, 7.168074330099288183 ) ;
#10170 = CONICAL_SURFACE ( 'NONE', #12260, 4.025000000000000355, 0.7853981633975870569 ) ;
#10171 = LINE ( 'NONE', #7189, #3087 ) ;
#10172 = CARTESIAN_POINT ( 'NONE',  ( -66.51364668169603078, 112.0410723289543995, -28.00000000000000355 ) ) ;
#10173 = DIRECTION ( 'NONE',  ( 0.3420201433256649937, 0.9396926207859097602, -0.000000000000000000 ) ) ;
#10174 = DIRECTION ( 'NONE',  ( 1.156482317317869999E-16, 0.000000000000000000, 1.000000000000000000 ) ) ;
#10175 = DIRECTION ( 'NONE',  ( 0.000000000000000000, -5.551115123125748189E-17, -1.000000000000000000 ) ) ;
#10176 = VERTEX_POINT ( 'NONE', #4778 ) ;
#10177 = EDGE_CURVE ( 'NONE', #14012, #14712, #1801, .T. ) ;
#10178 = PRESENTATION_LAYER_ASSIGNMENT (  '', '', ( #14077 ) ) ;
#10179 = EDGE_CURVE ( 'NONE', #2688, #17079, #15007, .T. ) ;
#10180 = CARTESIAN_POINT ( 'NONE',  ( -71.24615306438097662, 56.23601976522923707, -167.1454815528550739 ) ) ;
#10181 = DIRECTION ( 'NONE',  ( 1.000000000000000000, 0.000000000000000000, 0.000000000000000000 ) ) ;
#10182 = LINE ( 'NONE', #2816, #13911 ) ;
#10183 = CARTESIAN_POINT ( 'NONE',  ( -107.5676225674731938, 110.5691553257988460, 30.35917033480641791 ) ) ;
#10184 = ORIENTED_EDGE ( 'NONE', *, *, #4315, .F. ) ;
#10185 = AXIS2_PLACEMENT_3D ( 'NONE', #9435, #6516, #12232 ) ;
#10186 = CARTESIAN_POINT ( 'NONE',  ( -65.16279959635889441, 77.92691374209478283, -15.00000000000001243 ) ) ;
#10187 = CIRCLE ( 'NONE', #9294, 20.99999999999999645 ) ;
#10188 = CARTESIAN_POINT ( 'NONE',  ( -57.08002265617300708, 84.22855780814606419, 77.50000000000000000 ) ) ;
#10189 = ORIENTED_EDGE ( 'NONE', *, *, #11891, .T. ) ;
#10190 = EDGE_CURVE ( 'NONE', #11788, #18251, #4845, .T. ) ;
#10191 = CARTESIAN_POINT ( 'NONE',  ( -38.09490121289055509, 73.26749283227019305, 102.5000000000000000 ) ) ;
#10192 = CARTESIAN_POINT ( 'NONE',  ( -71.24615306438103346, 43.66964916522919538, -167.1454815528550739 ) ) ;
#10193 = ORIENTED_EDGE ( 'NONE', *, *, #17381, .F. ) ;
#10194 = ADVANCED_FACE ( 'NONE', ( #17596 ), #6094, .T. ) ;
#10195 = ORIENTED_EDGE ( 'NONE', *, *, #14773, .F. ) ;
#10196 = EDGE_CURVE ( 'NONE', #11754, #15862, #5913, .T. ) ;
#10197 = EDGE_CURVE ( 'NONE', #6984, #15061, #13322, .T. ) ;
#10198 = VERTEX_POINT ( 'NONE', #3033 ) ;
#10199 = CIRCLE ( 'NONE', #2126, 12.49999999999999112 ) ;
#10200 = CIRCLE ( 'NONE', #6594, 4.600000000000006750 ) ;
#10201 = PLANE ( 'NONE',  #10901 ) ;
#10202 = CARTESIAN_POINT ( 'NONE',  ( -102.5926225674731853, 102.8748711238780373, 20.00000000000000355 ) ) ;
#10203 = CARTESIAN_POINT ( 'NONE',  ( -68.99615306438103346, 32.81108233166271759, -15.00000000000001421 ) ) ;
#10204 = ADVANCED_FACE ( 'NONE', ( #11828 ), #1900, .F. ) ;
#10205 = CARTESIAN_POINT ( 'NONE',  ( -71.24615306438073503, 129.3815214545637104, -167.1454815528550739 ) ) ;
#10206 = DIRECTION ( 'NONE',  ( -0.9396926207859084279, 0.3420201433256686574, -4.890320548438448905E-16 ) ) ;
#10207 = VERTEX_POINT ( 'NONE', #7345 ) ;
#10208 = CARTESIAN_POINT ( 'NONE',  ( -68.99615306438111872, 20.85956758813031797, -15.00000000000001421 ) ) ;
#10209 = CIRCLE ( 'NONE', #13788, 4.600000000000006750 ) ;
#10210 = DIRECTION ( 'NONE',  ( 0.9396926207859158664, 0.3420201433256481738, -1.086737899652998397E-16 ) ) ;
#10211 = CARTESIAN_POINT ( 'NONE',  ( -53.29103256796045684, 73.45256821284057480, -167.1454815528550739 ) ) ;
#10212 = ORIENTED_EDGE ( 'NONE', *, *, #9838, .T. ) ;
#10213 = AXIS2_PLACEMENT_3D ( 'NONE', #18266, #15077, #17116 ) ;
#10214 = DIRECTION ( 'NONE',  ( 0.000000000000000000, 0.000000000000000000, -1.000000000000000000 ) ) ;
#10215 = VECTOR ( 'NONE', #11537, 1000.000000000000000 ) ;
#10216 = CARTESIAN_POINT ( 'NONE',  ( -110.5389732269433978, -91.12516209206943074, -10.00231928999220621 ) ) ;
#10217 = ORIENTED_EDGE ( 'NONE', *, *, #12500, .T. ) ;
#10218 = ORIENTED_EDGE ( 'NONE', *, *, #7560, .T. ) ;
#10219 = B_SPLINE_CURVE_WITH_KNOTS ( 'NONE', 3,
 ( #16474, #2080, #17512, #10407, #16096, #10602 ),
 .UNSPECIFIED., .F., .F.,
 ( 4, 2, 4 ),
 ( 0.007841539089391896464, 0.008626660956717931844, 0.009411782824043968959 ),
 .UNSPECIFIED. ) ;
#10220 = VECTOR ( 'NONE', #245, 1000.000000000000000 ) ;
#10221 = CARTESIAN_POINT ( 'NONE',  ( -64.09025127992791226, 117.8748711238780373, 35.00000000000000000 ) ) ;
#10222 = LINE ( 'NONE', #14346, #5802 ) ;
#10223 = LINE ( 'NONE', #33, #11145 ) ;
#10224 = VERTEX_POINT ( 'NONE', #13059 ) ;
#10225 = VECTOR ( 'NONE', #9997, 1000.000000000000000 ) ;
#10226 = CIRCLE ( 'NONE', #12643, 45.40389983439752086 ) ;
#10227 = ORIENTED_EDGE ( 'NONE', *, *, #10660, .T. ) ;
#10228 = CARTESIAN_POINT ( 'NONE',  ( -50.90853507983961634, 93.09943318379598054, 15.00000000000006928 ) ) ;
#10229 = CARTESIAN_POINT ( 'NONE',  ( -123.4618227840623632, -111.0842361345572158, 57.00000000000000000 ) ) ;
#10230 = CARTESIAN_POINT ( 'NONE',  ( -71.24615306438091977, 71.94398301522919326, -15.00000000000001421 ) ) ;
#10231 = CARTESIAN_POINT ( 'NONE',  ( -68.99615306438093398, 45.99230878813023793, 15.00000000000006928 ) ) ;
#10232 = ORIENTED_EDGE ( 'NONE', *, *, #642, .F. ) ;
#10233 = CARTESIAN_POINT ( 'NONE',  ( -68.99615306438067819, 145.9084177316626949, -167.1454815528550739 ) ) ;
#10235 = EDGE_LOOP ( 'NONE', ( #1611, #15089, #2319, #8672 ) ) ;
#10234 = PRODUCT_RELATED_PRODUCT_CATEGORY ( 'part', '', ( #6380 ) ) ;
#10236 = AXIS2_PLACEMENT_3D ( 'NONE', #14529, #7241, #17320 ) ;
#10237 = EDGE_LOOP ( 'NONE', ( #11433, #12213, #7303, #17229 ) ) ;
#10238 = AXIS2_PLACEMENT_3D ( 'NONE', #12378, #853, #5051 ) ;
#10239 = ORIENTED_EDGE ( 'NONE', *, *, #14454, .F. ) ;
#10240 = DIRECTION ( 'NONE',  ( 1.000000000000000000, -0.000000000000000000, -0.000000000000000000 ) ) ;
#10241 = CARTESIAN_POINT ( 'NONE',  ( -67.59262256747317110, 61.64996188551982215, 25.00000000000000355 ) ) ;
#10242 = DIRECTION ( 'NONE',  ( 0.000000000000000000, 1.000000000000000000, 0.000000000000000000 ) ) ;
#10243 = AXIS2_PLACEMENT_3D ( 'NONE', #16288, #572, #855 ) ;
#10244 = EDGE_LOOP ( 'NONE', ( #3717, #10438, #5556, #10110 ) ) ;
#10245 = CARTESIAN_POINT ( 'NONE',  ( -71.24615306438076345, 122.2094654152292037, -15.00000000000001421 ) ) ;
#10246 = FACE_OUTER_BOUND ( 'NONE', #15086, .T. ) ;
#10247 = DIRECTION ( 'NONE',  ( 0.9396926207859157554, 0.3420201433256481738, 4.890320548438487362E-16 ) ) ;
#10248 = LINE ( 'NONE', #13077, #15965 ) ;
#10249 = ORIENTED_EDGE ( 'NONE', *, *, #3325, .T. ) ;
#10250 = DIRECTION ( 'NONE',  ( -5.204170427930409450E-16, 0.000000000000000000, 1.000000000000000000 ) ) ;
#10251 = CIRCLE ( 'NONE', #10539, 11.04359719766049430 ) ;
#10252 = VECTOR ( 'NONE', #384, 1000.000000000000000 ) ;
#10253 = CIRCLE ( 'NONE', #2181, 42.49926016645017057 ) ;
#10254 = DIRECTION ( 'NONE',  ( 0.000000000000000000, 0.000000000000000000, 1.000000000000000000 ) ) ;
#10255 = CARTESIAN_POINT ( 'NONE',  ( -70.06856178257687873, 57.88796029049330372, 22.35917033480642502 ) ) ;
#10257 = VERTEX_POINT ( 'NONE', #4612 ) ;
#10256 = EDGE_CURVE ( 'NONE', #12606, #9020, #17327, .T. ) ;
#10258 = DIRECTION ( 'NONE',  ( 1.000000000000000000, 0.000000000000000000, 0.000000000000000000 ) ) ;
#10259 = DIRECTION ( 'NONE',  ( 1.000000000000000000, -0.000000000000000000, -0.000000000000000000 ) ) ;
#10260 = EDGE_LOOP ( 'NONE', ( #9453, #16121, #16986, #10889, #12736, #16620, #9568, #1363, #5916, #18078, #12569, #15872 ) ) ;
#10261 = VERTEX_POINT ( 'NONE', #14537 ) ;
#10262 = ADVANCED_FACE ( 'NONE', ( #1713 ), #10332, .T. ) ;
#10263 = VECTOR ( 'NONE', #17854, 1000.000000000000000 ) ;
#10264 = AXIS2_PLACEMENT_3D ( 'NONE', #16896, #9594, #14198 ) ;
#10265 = VERTEX_POINT ( 'NONE', #9470 ) ;
#10266 = DIRECTION ( 'NONE',  ( 1.000000000000000000, -0.000000000000000000, -0.000000000000000000 ) ) ;
#10267 = DIRECTION ( 'NONE',  ( 0.000000000000000000, -0.01622727141748259855, 0.9998683291625671821 ) ) ;
#10268 = DIRECTION ( 'NONE',  ( -1.000000000000000000, 0.000000000000000000, 0.000000000000000000 ) ) ;
#10269 = CARTESIAN_POINT ( 'NONE',  ( -67.59262256747317110, 57.88796029049329661, -26.35917033480641436 ) ) ;
#10270 = DIRECTION ( 'NONE',  ( 1.000000000000000000, -0.000000000000000000, -0.000000000000000000 ) ) ;
#10271 = LINE ( 'NONE', #3244, #7886 ) ;
#10272 = ORIENTED_EDGE ( 'NONE', *, *, #8376, .T. ) ;
#10273 = AXIS2_PLACEMENT_3D ( 'NONE', #6012, #12981, #1646 ) ;
#10274 = CYLINDRICAL_SURFACE ( 'NONE', #4212, 4.600000000000006750 ) ;
#10275 = CARTESIAN_POINT ( 'NONE',  ( -68.99615306438111872, 7.678341131662687502, -15.00000000000001421 ) ) ;
#10276 = LINE ( 'NONE', #7650, #1657 ) ;
#10277 = CYLINDRICAL_SURFACE ( 'NONE', #7244, 4.599999999999992539 ) ;
#10278 = CARTESIAN_POINT ( 'NONE',  ( -37.17496177488503406, 91.05728076224789902, 59.38899799626690168 ) ) ;
#10279 = PRODUCT_DEFINITION_FORMATION_WITH_SPECIFIED_SOURCE ( 'ANY', '', #5524, .NOT_KNOWN. ) ;
#10280 = VECTOR ( 'NONE', #17829, 1000.000000000000000 ) ;
#10281 = VECTOR ( 'NONE', #4245, 1000.000000000000114 ) ;
#10282 = DIRECTION ( 'NONE',  ( 0.000000000000000000, 0.000000000000000000, 1.000000000000000000 ) ) ;
#10283 = ORIENTED_EDGE ( 'NONE', *, *, #8189, .F. ) ;
#10284 = DIRECTION ( 'NONE',  ( -0.9396926207859084279, 0.3420201433256689905, 0.000000000000000000 ) ) ;
#10285 = ORIENTED_EDGE ( 'NONE', *, *, #18438, .T. ) ;
#10286 = ORIENTED_EDGE ( 'NONE', *, *, #10071, .F. ) ;
#10287 = ADVANCED_FACE ( 'NONE', ( #17796 ), #682, .F. ) ;
#10288 = TOROIDAL_SURFACE ( 'NONE', #18370, 10.65431531532568243, 5.000000000000000000 ) ;
#10289 = EDGE_CURVE ( 'NONE', #17556, #3227, #10495, .T. ) ;
#10290 = AXIS2_PLACEMENT_3D ( 'NONE', #5973, #6339, #16073 ) ;
#10291 = EDGE_CURVE ( 'NONE', #17316, #14280, #13527, .T. ) ;
#10292 = ORIENTED_EDGE ( 'NONE', *, *, #13245, .F. ) ;
#10293 = VECTOR ( 'NONE', #1821, 1000.000000000000000 ) ;
#10294 = CIRCLE ( 'NONE', #5819, 4.000000000000003553 ) ;
#10295 = FACE_OUTER_BOUND ( 'NONE', #18056, .T. ) ;
#10296 = DIRECTION ( 'NONE',  ( 0.000000000000000000, 1.000000000000000000, 0.000000000000000000 ) ) ;
#10297 = CARTESIAN_POINT ( 'NONE',  ( -76.88577610500824733, 77.11479169650115750, 60.07327016997842151 ) ) ;
#10298 = DIRECTION ( 'NONE',  ( -0.9396926207859069846, 0.3420201433256723766, -4.890320548438442003E-16 ) ) ;
#10299 = CARTESIAN_POINT ( 'NONE',  ( -127.5926225674731995, 110.5691553257988460, 26.35917033480641436 ) ) ;
#10300 = EDGE_CURVE ( 'NONE', #9028, #7250, #11739, .T. ) ;
#10301 = CARTESIAN_POINT ( 'NONE',  ( -68.99615306438077766, 117.6340838816626899, 15.00000000000006928 ) ) ;
#10302 = EDGE_LOOP ( 'NONE', ( #13881, #12546, #4928, #17510 ) ) ;
#10303 = EDGE_CURVE ( 'NONE', #12950, #6650, #17978, .T. ) ;
#10304 = EDGE_CURVE ( 'NONE', #4587, #10505, #5063, .T. ) ;
#10305 = VECTOR ( 'NONE', #12177, 999.9999999999998863 ) ;
#10306 = FACE_OUTER_BOUND ( 'NONE', #2871, .T. ) ;
#10307 = CARTESIAN_POINT ( 'NONE',  ( -76.37409655828280108, -96.08423613455721579, 45.05044770573179846 ) ) ;
#10308 = EDGE_CURVE ( 'NONE', #7586, #5881, #16424, .T. ) ;
#10309 = FACE_OUTER_BOUND ( 'NONE', #11017, .T. ) ;
#10310 = VERTEX_POINT ( 'NONE', #16381 ) ;
#10311 = VECTOR ( 'NONE', #4189, 1000.000000000000000 ) ;
#10312 = CARTESIAN_POINT ( 'NONE',  ( -65.41598826576338865, 91.10542963993673027, -15.00000000000001421 ) ) ;
#10313 = CIRCLE ( 'NONE', #5226, 18.23991632971910803 ) ;
#10314 = LINE ( 'NONE', #1435, #15168 ) ;
#10316 = ORIENTED_EDGE ( 'NONE', *, *, #9516, .F. ) ;
#10315 = AXIS2_PLACEMENT_3D ( 'NONE', #3603, #623, #2210 ) ;
#10317 = EDGE_CURVE ( 'NONE', #9318, #8476, #3669, .T. ) ;
#10318 = ADVANCED_FACE ( 'NONE', ( #14978 ), #16298, .T. ) ;
#10319 = EDGE_CURVE ( 'NONE', #7713, #10372, #15079, .T. ) ;
#10320 = ORIENTED_EDGE ( 'NONE', *, *, #14526, .F. ) ;
#10321 = DIRECTION ( 'NONE',  ( 0.000000000000000000, 1.000000000000000000, 0.000000000000000000 ) ) ;
#10322 = CARTESIAN_POINT ( 'NONE',  ( -57.08002265617300708, 84.22855780814606419, -15.00000000000001421 ) ) ;
#10323 = CARTESIAN_POINT ( 'NONE',  ( -68.99615306438089135, 83.69142058813029905, -167.1454815528550739 ) ) ;
#10324 = VECTOR ( 'NONE', #1182, 1000.000000000000000 ) ;
#10325 = ORIENTED_EDGE ( 'NONE', *, *, #17540, .T. ) ;
#10326 = AXIS2_PLACEMENT_3D ( 'NONE', #7199, #12822, #7031 ) ;
#10327 = AXIS2_PLACEMENT_3D ( 'NONE', #7649, #4730, #10450 ) ;
#10328 = ORIENTED_EDGE ( 'NONE', *, *, #14943, .T. ) ;
#10329 = LINE ( 'NONE', #1709, #9588 ) ;
#10330 = CARTESIAN_POINT ( 'NONE',  ( -36.03642545851251100, 84.22855780814606419, 77.50000000000000000 ) ) ;
#10331 = DIRECTION ( 'NONE',  ( -1.000000000000000000, 0.000000000000000000, 1.387778780781446662E-16 ) ) ;
#10332 = CYLINDRICAL_SURFACE ( 'NONE', #9643, 45.40389983439752086 ) ;
#10333 = ORIENTED_EDGE ( 'NONE', *, *, #9138, .T. ) ;
#10334 = EDGE_CURVE ( 'NONE', #16663, #9751, #17695, .T. ) ;
#10335 = EDGE_CURVE ( 'NONE', #703, #2929, #13821, .T. ) ;
#10336 = DIRECTION ( 'NONE',  ( 0.000000000000000000, 0.000000000000000000, 1.000000000000000000 ) ) ;
#10337 = ORIENTED_EDGE ( 'NONE', *, *, #8100, .T. ) ;
#10338 = CARTESIAN_POINT ( 'NONE',  ( 0.000000000000000000, 0.000000000000000000, 0.000000000000000000 ) ) ;
#10339 = VERTEX_POINT ( 'NONE', #12677 ) ;
#10340 = VERTEX_POINT ( 'NONE', #5343 ) ;
#10341 = LINE ( 'NONE', #7623, #3409 ) ;
#10342 = DIRECTION ( 'NONE',  ( 0.000000000000000000, 0.000000000000000000, 1.000000000000000000 ) ) ;
#10343 = ORIENTED_EDGE ( 'NONE', *, *, #17806, .F. ) ;
#10344 = LINE ( 'NONE', #17526, #13412 ) ;
#10345 = CARTESIAN_POINT ( 'NONE',  ( -66.96222586426215173, 88.60139997190893268, -167.1454815528550739 ) ) ;
#10346 = DIRECTION ( 'NONE',  ( -0.000000000000000000, -0.000000000000000000, 1.000000000000000000 ) ) ;
#10347 = VERTEX_POINT ( 'NONE', #13972 ) ;
#10348 = LINE ( 'NONE', #15957, #14381 ) ;
#10349 = FACE_OUTER_BOUND ( 'NONE', #5421, .T. ) ;
#10350 = DIRECTION ( 'NONE',  ( 0.9396926207859110924, 0.3420201433256612189, 4.890320548438462711E-16 ) ) ;
#10351 = VERTEX_POINT ( 'NONE', #8350 ) ;
#10352 = DIRECTION ( 'NONE',  ( 0.000000000000000000, 1.000000000000000000, 0.000000000000000000 ) ) ;
#10353 = DIRECTION ( 'NONE',  ( 0.000000000000000000, 0.000000000000000000, 1.000000000000000000 ) ) ;
#10354 = VERTEX_POINT ( 'NONE', #15267 ) ;
#10355 = VERTEX_POINT ( 'NONE', #5262 ) ;
#10356 = EDGE_LOOP ( 'NONE', ( #5552, #3295, #10090, #8446 ) ) ;
#10358 = EDGE_CURVE ( 'NONE', #17780, #8931, #4061, .T. ) ;
#10357 = CARTESIAN_POINT ( 'NONE',  ( -46.36441787118067026, 82.83016482797245317, -167.1454815528550739 ) ) ;
#10359 = ORIENTED_EDGE ( 'NONE', *, *, #4814, .T. ) ;
#10360 = CARTESIAN_POINT ( 'NONE',  ( 0.000000000000000000, 0.000000000000000000, 0.000000000000000000 ) ) ;
#10361 = CYLINDRICAL_SURFACE ( 'NONE', #5227, 4.599999999999999645 ) ;
#10362 = FACE_OUTER_BOUND ( 'NONE', #1190, .T. ) ;
#10363 = DIRECTION ( 'NONE',  ( 0.000000000000000000, 0.000000000000000000, -1.000000000000000000 ) ) ;
#10364 = CARTESIAN_POINT ( 'NONE',  ( 15.23320273812466041, 0.000000000000000000, -3.000000000000000000 ) ) ;
#10365 = ORIENTED_EDGE ( 'NONE', *, *, #14546, .T. ) ;
#10366 = LINE ( 'NONE', #11770, #16412 ) ;
#10367 = DIRECTION ( 'NONE',  ( 1.000000000000000000, 0.000000000000000000, 0.000000000000000000 ) ) ;
#10368 = DIRECTION ( 'NONE',  ( 0.000000000000000000, 0.000000000000000000, 1.000000000000000000 ) ) ;
#10369 = CARTESIAN_POINT ( 'NONE',  ( -58.51182448057780050, 96.64628479562776420, -15.00000000000001421 ) ) ;
#10370 = DIRECTION ( 'NONE',  ( -1.000000000000000000, 6.550315845288414753E-14, 1.387778780781443703E-16 ) ) ;
#10371 = FACE_OUTER_BOUND ( 'NONE', #2747, .T. ) ;
#10372 = VERTEX_POINT ( 'NONE', #11351 ) ;
#10373 = DIRECTION ( 'NONE',  ( -1.000000000000000000, -0.000000000000000000, -0.000000000000000000 ) ) ;
#10374 = CARTESIAN_POINT ( 'NONE',  ( -36.03642545851251811, 83.72858089318386021, 55.00000000000002132 ) ) ;
#10375 = ORIENTED_EDGE ( 'NONE', *, *, #15664, .T. ) ;
#10376 = ORIENTED_EDGE ( 'NONE', *, *, #9703, .T. ) ;
#10377 = ORIENTED_EDGE ( 'NONE', *, *, #14438, .F. ) ;
#10378 = CARTESIAN_POINT ( 'NONE',  ( 0.05533025579362366858, 4.993776679985823641, 4.350525068611912793 ) ) ;
#10379 = CARTESIAN_POINT ( 'NONE',  ( 9.543663295069050534, 56.41207303426870112, 7.000000000000010658 ) ) ;
#10380 = LINE ( 'NONE', #3263, #1480 ) ;
#10381 = DIRECTION ( 'NONE',  ( 0.9396926207859084279, 0.3420201433256686574, -1.086737899652989892E-16 ) ) ;
#10382 = DIRECTION ( 'NONE',  ( 0.000000000000000000, 0.000000000000000000, 1.000000000000000000 ) ) ;
#10383 = CARTESIAN_POINT ( 'NONE',  ( -68.99615306438072082, 127.6737176881302958, -167.1454815528550739 ) ) ;
#10384 = CARTESIAN_POINT ( 'NONE',  ( -68.99615306438094819, 64.84186468813030046, -167.1454815528550739 ) ) ;
#10385 = ORIENTED_EDGE ( 'NONE', *, *, #7552, .F. ) ;
#10386 = CARTESIAN_POINT ( 'NONE',  ( -59.35080917176598092, 94.79374675277695417, 15.00000000000006928 ) ) ;
#10387 = ADVANCED_FACE ( 'NONE', ( #2739 ), #9561, .T. ) ;
#10388 = CARTESIAN_POINT ( 'NONE',  ( -77.14491745292085056, -93.39009998357852282, 44.16867553823936277 ) ) ;
#10389 =( REPRESENTATION_RELATIONSHIP ('NONE','NONE', #359, #5501 ) REPRESENTATION_RELATIONSHIP_WITH_TRANSFORMATION ( #11553 )SHAPE_REPRESENTATION_RELATIONSHIP( ) );
#10390 = CARTESIAN_POINT ( 'NONE',  ( -71.24615306438080609, 103.3599095152292193, 15.00000000000006928 ) ) ;
#10391 = VERTEX_POINT ( 'NONE', #12851 ) ;
#10392 = CARTESIAN_POINT ( 'NONE',  ( -57.08002265617300708, 84.22855780814606419, -167.1454815528550739 ) ) ;
#10393 = LINE ( 'NONE', #13212, #5919 ) ;
#10394 = ORIENTED_EDGE ( 'NONE', *, *, #13828, .T. ) ;
#10395 = VECTOR ( 'NONE', #9188, 1000.000000000000000 ) ;
#10396 = EDGE_CURVE ( 'NONE', #11747, #11084, #13879, .T. ) ;
#10397 = ORIENTED_EDGE ( 'NONE', *, *, #1820, .F. ) ;
#10398 = EDGE_CURVE ( 'NONE', #9366, #14319, #18320, .T. ) ;
#10399 = LINE ( 'NONE', #10221, #15971 ) ;
#10400 = LINE ( 'NONE', #17684, #4888 ) ;
#10401 = CARTESIAN_POINT ( 'NONE',  ( -68.99615306438100504, 39.70912348813028103, -167.1454815528550739 ) ) ;
#10402 = ORIENTED_EDGE ( 'NONE', *, *, #6767, .T. ) ;
#10403 = EDGE_LOOP ( 'NONE', ( #12778, #16656, #10599, #17802 ) ) ;
#10404 = AXIS2_PLACEMENT_3D ( 'NONE', #10787, #12107, #15085 ) ;
#10405 = EDGE_CURVE ( 'NONE', #18141, #18474, #9663, .T. ) ;
#10406 = CARTESIAN_POINT ( 'NONE',  ( -71.24615306438097662, 59.37761241522920841, -167.1454815528550739 ) ) ;
#10407 = CARTESIAN_POINT ( 'NONE',  ( -66.05502429040123502, 111.0949457325500163, 25.00000000000000355 ) ) ;
#10408 = CARTESIAN_POINT ( 'NONE',  ( -65.06546592763127990, -91.08423613455721579, -2.621725226070001387E-13 ) ) ;
#10409 = EDGE_CURVE ( 'NONE', #4575, #6976, #394, .T. ) ;
#10410 = CARTESIAN_POINT ( 'NONE',  ( -71.24615306438076345, 125.3510580652292248, -15.00000000000001421 ) ) ;
#10411 = EDGE_CURVE ( 'NONE', #12287, #6666, #6054, .T. ) ;
#10412 = ORIENTED_EDGE ( 'NONE', *, *, #2178, .F. ) ;
#10413 = DIRECTION ( 'NONE',  ( -0.000000000000000000, -0.000000000000000000, -1.000000000000000000 ) ) ;
#10414 = ORIENTED_EDGE ( 'NONE', *, *, #5149, .T. ) ;
#10415 = DIRECTION ( 'NONE',  ( 1.000000000000000000, -0.000000000000000000, -0.000000000000000000 ) ) ;
#10416 = ORIENTED_EDGE ( 'NONE', *, *, #3410, .T. ) ;
#10417 = ADVANCED_FACE ( 'NONE', ( #18174 ), #16755, .T. ) ;
#10418 = CIRCLE ( 'NONE', #9512, 5.654315315325680658 ) ;
#10419 = ORIENTED_EDGE ( 'NONE', *, *, #309, .F. ) ;
#10420 = EDGE_CURVE ( 'NONE', #1022, #8464, #1432, .T. ) ;
#10421 = CARTESIAN_POINT ( 'NONE',  ( -68.99615306438096241, 33.42593818813026729, 15.00000000000006928 ) ) ;
#10422 = ADVANCED_FACE ( 'NONE', ( #16956 ), #9944, .T. ) ;
#10423 = DIRECTION ( 'NONE',  ( -1.000000000000000000, 0.000000000000000000, 0.000000000000000000 ) ) ;
#10424 = VERTEX_POINT ( 'NONE', #18270 ) ;
#10425 = CARTESIAN_POINT ( 'NONE',  ( -71.24615306438069240, 135.6647067545637242, -15.00000000000001421 ) ) ;
#10426 = LINE ( 'NONE', #8764, #10796 ) ;
#10427 = CARTESIAN_POINT ( 'NONE',  ( -71.24615306438103346, 44.55851990456372391, -167.1454815528550739 ) ) ;
#10428 = VERTEX_POINT ( 'NONE', #10975 ) ;
#10429 = EDGE_CURVE ( 'NONE', #15321, #12181, #1349, .T. ) ;
#10430 = FACE_OUTER_BOUND ( 'NONE', #11953, .T. ) ;
#10431 = AXIS2_PLACEMENT_3D ( 'NONE', #11393, #6893, #9891 ) ;
#10432 = FACE_OUTER_BOUND ( 'NONE', #5931, .T. ) ;
#10433 = DIRECTION ( 'NONE',  ( 0.000000000000000000, 0.000000000000000000, 1.000000000000000000 ) ) ;
#10434 = VERTEX_POINT ( 'NONE', #11168 ) ;
#10435 = AXIS2_PLACEMENT_3D ( 'NONE', #6121, #14478, #1567 ) ;
#10436 = DIRECTION ( 'NONE',  ( 0.000000000000000000, 1.000000000000000000, 0.000000000000000000 ) ) ;
#10437 = LINE ( 'NONE', #1929, #6234 ) ;
#10438 = ORIENTED_EDGE ( 'NONE', *, *, #10179, .T. ) ;
#10439 = ORIENTED_EDGE ( 'NONE', *, *, #17822, .T. ) ;
#10440 = ORIENTED_EDGE ( 'NONE', *, *, #2010, .T. ) ;
#10441 = VECTOR ( 'NONE', #11475, 1000.000000000000000 ) ;
#10442 = CARTESIAN_POINT ( 'NONE',  ( -57.08002265617300708, 84.22855780814606419, 15.00000000000006928 ) ) ;
#10443 = VECTOR ( 'NONE', #11439, 1000.000000000000000 ) ;
#10444 = DIRECTION ( 'NONE',  ( 0.000000000000000000, 0.000000000000000000, 1.000000000000000000 ) ) ;
#10445 = FACE_OUTER_BOUND ( 'NONE', #3678, .T. ) ;
#10446 =( LENGTH_UNIT ( ) NAMED_UNIT ( * ) SI_UNIT ( .MILLI., .METRE. ) );
#10447 = CARTESIAN_POINT ( 'NONE',  ( -31.03642545851250745, 84.22855780814606419, 37.50000000000000000 ) ) ;
#10448 = CARTESIAN_POINT ( 'NONE',  ( -57.08002265617300708, 84.22855780814606419, -15.00000000000001421 ) ) ;
#10449 = CARTESIAN_POINT ( 'NONE',  ( -71.24615306438109030, 31.99214930456376038, -167.1454815528550739 ) ) ;
#10450 = DIRECTION ( 'NONE',  ( 0.000000000000000000, 0.000000000000000000, -1.000000000000000000 ) ) ;
#10451 = DIRECTION ( 'NONE',  ( 1.156482317317869999E-16, 0.000000000000000000, 1.000000000000000000 ) ) ;
#10452 = FACE_OUTER_BOUND ( 'NONE', #12448, .T. ) ;
#10453 = CARTESIAN_POINT ( 'NONE',  ( -36.80510220921193820, 89.87539756129703505, 57.54020390674075713 ) ) ;
#10454 = VERTEX_POINT ( 'NONE', #16859 ) ;
#10455 = DIRECTION ( 'NONE',  ( 1.000000000000000000, 0.000000000000000000, 5.551115123125780730E-16 ) ) ;
#10456 = VECTOR ( 'NONE', #14434, 1000.000000000000000 ) ;
#10457 = ORIENTED_EDGE ( 'NONE', *, *, #14970, .F. ) ;
#10458 = DIRECTION ( 'NONE',  ( 1.000000000000000000, 0.000000000000000000, 3.771137991253928573E-16 ) ) ;
#10459 = VECTOR ( 'NONE', #14946, 1000.000000000000114 ) ;
#10460 = DIRECTION ( 'NONE',  ( -0.000000000000000000, 1.200240087506842815E-16, 1.000000000000000000 ) ) ;
#10461 = VERTEX_POINT ( 'NONE', #15464 ) ;
#10462 = AXIS2_PLACEMENT_3D ( 'NONE', #11427, #4125, #16939 ) ;
#10463 = EDGE_LOOP ( 'NONE', ( #7086, #5793, #5914, #1788 ) ) ;
#10464 = ORIENTED_EDGE ( 'NONE', *, *, #15322, .T. ) ;
#10465 = DIRECTION ( 'NONE',  ( 0.000000000000000000, 0.000000000000000000, 1.000000000000000000 ) ) ;
#10466 = DIRECTION ( 'NONE',  ( -1.000000000000000000, -2.062304371594500740E-16, 0.000000000000000000 ) ) ;
#10467 = AXIS2_PLACEMENT_3D ( 'NONE', #6740, #8036, #1044 ) ;
#10468 = DIRECTION ( 'NONE',  ( 0.000000000000000000, 0.000000000000000000, 1.000000000000000000 ) ) ;
#10469 = CARTESIAN_POINT ( 'NONE',  ( -64.09025127992788384, 50.58224449241409104, -35.00000000000000000 ) ) ;
#10470 = AXIS2_PLACEMENT_3D ( 'NONE', #5011, #9428, #13444 ) ;
#10471 = FACE_OUTER_BOUND ( 'NONE', #247, .T. ) ;
#10472 = DIRECTION ( 'NONE',  ( -1.000000000000000000, -0.000000000000000000, -0.000000000000000000 ) ) ;
#10473 = ORIENTED_EDGE ( 'NONE', *, *, #13183, .F. ) ;
#10474 = DIRECTION ( 'NONE',  ( 0.000000000000000000, 0.5000000000000009992, 0.8660254037844381525 ) ) ;
#10475 = DIRECTION ( 'NONE',  ( -1.000000000000000000, -2.062304371594500740E-16, -0.000000000000000000 ) ) ;
#10476 = CARTESIAN_POINT ( 'NONE',  ( -127.5926225674732279, 187.7866419848965052, 15.00000000000004263 ) ) ;
#10477 = ORIENTED_EDGE ( 'NONE', *, *, #9560, .F. ) ;
#10478 = VECTOR ( 'NONE', #11373, 1000.000000000000000 ) ;
#10479 = FACE_OUTER_BOUND ( 'NONE', #6747, .T. ) ;
#10480 = CARTESIAN_POINT ( 'NONE',  ( -67.50540723371459251, 87.07303407725210320, -167.1454815528550739 ) ) ;
#10481 = EDGE_LOOP ( 'NONE', ( #7078, #1903, #1768, #1234 ) ) ;
#10482 = AXIS2_PLACEMENT_3D ( 'NONE', #3031, #3128, #42 ) ;
#10483 = VECTOR ( 'NONE', #3867, 1000.000000000000000 ) ;
#10484 = VERTEX_POINT ( 'NONE', #12769 ) ;
#10485 = EDGE_CURVE ( 'NONE', #8500, #6562, #18467, .T. ) ;
#10486 = CARTESIAN_POINT ( 'NONE',  ( -67.59262256747319952, 111.6514400295689171, 22.50837044127971254 ) ) ;
#10487 = CARTESIAN_POINT ( 'NONE',  ( -57.08002265617300708, 84.22855780814606419, -28.00000000000000355 ) ) ;
#10488 = CARTESIAN_POINT ( 'NONE',  ( 0.000000000000000000, 0.000000000000000000, 0.000000000000000000 ) ) ;
#10489 = ORIENTED_EDGE ( 'NONE', *, *, #2657, .F. ) ;
#10490 = CIRCLE ( 'NONE', #2135, 4.599999999999992539 ) ;
#10491 = ORIENTED_EDGE ( 'NONE', *, *, #14729, .T. ) ;
#10492 = CARTESIAN_POINT ( 'NONE',  ( 7.512335209198389707E-14, -5.309483803148955516, -3.803704290982263814 ) ) ;
#10493 = DIRECTION ( 'NONE',  ( -1.156482317317869999E-16, 0.000000000000000000, -1.000000000000000000 ) ) ;
#10494 = CARTESIAN_POINT ( 'NONE',  ( -77.78632074013589204, 88.00379445693184266, 56.00117480735330133 ) ) ;
#10495 = LINE ( 'NONE', #863, #14432 ) ;
#10496 = AXIS2_PLACEMENT_3D ( 'NONE', #17975, #15263, #94 ) ;
#10497 = VECTOR ( 'NONE', #12, 1000.000000000000000 ) ;
#10498 = ORIENTED_EDGE ( 'NONE', *, *, #4337, .F. ) ;
#10499 = EDGE_CURVE ( 'NONE', #11807, #13603, #16513, .T. ) ;
#10500 = FACE_OUTER_BOUND ( 'NONE', #13345, .T. ) ;
#10501 = ORIENTED_EDGE ( 'NONE', *, *, #1405, .T. ) ;
#10502 = LINE ( 'NONE', #16200, #18176 ) ;
#10503 = ORIENTED_EDGE ( 'NONE', *, *, #18058, .T. ) ;
#10504 = CIRCLE ( 'NONE', #14989, 5.654315315325680658 ) ;
#10505 = VERTEX_POINT ( 'NONE', #5545 ) ;
#10506 = VERTEX_POINT ( 'NONE', #8552 ) ;
#10507 = EDGE_CURVE ( 'NONE', #16077, #8426, #7137, .T. ) ;
#10508 = EDGE_CURVE ( 'NONE', #1230, #9843, #11614, .T. ) ;
#10509 = CIRCLE ( 'NONE', #2456, 3.999999999999989786 ) ;
#10510 = CIRCLE ( 'NONE', #14415, 20.99999999999998934 ) ;
#10511 = FILL_AREA_STYLE_COLOUR ( '', #8787 ) ;
#10512 = LINE ( 'NONE', #14813, #17393 ) ;
#10513 = ORIENTED_EDGE ( 'NONE', *, *, #3208, .F. ) ;
#10514 = DIRECTION ( 'NONE',  ( 1.000000000000000000, 0.000000000000000000, 0.000000000000000000 ) ) ;
#10515 = CARTESIAN_POINT ( 'NONE',  ( -46.10942163047475617, 78.23723799236688592, -15.00000000000001421 ) ) ;
#10516 = ORIENTED_EDGE ( 'NONE', *, *, #2899, .T. ) ;
#10517 = TOROIDAL_SURFACE ( 'NONE', #9338, 7.372635429264279061, 4.962965561209096599 ) ;
#10518 = DIRECTION ( 'NONE',  ( 1.000000000000000000, 0.000000000000000000, 0.000000000000000000 ) ) ;
#10519 = ORIENTED_EDGE ( 'NONE', *, *, #5828, .T. ) ;
#10520 = EDGE_CURVE ( 'NONE', #13807, #7544, #10121, .T. ) ;
#10521 = CARTESIAN_POINT ( 'NONE',  ( -46.38449965345759551, 85.77305660501679085, -167.1454815528550739 ) ) ;
#10522 = DIRECTION ( 'NONE',  ( 1.000000000000000000, 2.062304371594500494E-16, -0.000000000000000000 ) ) ;
#10523 = EDGE_LOOP ( 'NONE', ( #15477, #25, #9876, #8885 ) ) ;
#10524 = AXIS2_PLACEMENT_3D ( 'NONE', #3973, #13999, #1180 ) ;
#10525 = AXIS2_PLACEMENT_3D ( 'NONE', #16972, #12695, #9969 ) ;
#10526 = EDGE_CURVE ( 'NONE', #15988, #10428, #8994, .T. ) ;
#10527 = PLANE ( 'NONE',  #14766 ) ;
#10528 = EDGE_CURVE ( 'NONE', #11836, #9725, #7274, .T. ) ;
#10529 = CARTESIAN_POINT ( 'NONE',  ( -77.79035519103784679, -92.58100082067039693, -43.41642806912999930 ) ) ;
#10530 = VERTEX_POINT ( 'NONE', #10040 ) ;
#10531 = VERTEX_POINT ( 'NONE', #2927 ) ;
#10532 = EDGE_CURVE ( 'NONE', #8271, #2272, #14684, .T. ) ;
#10533 = VECTOR ( 'NONE', #15794, 1000.000000000000000 ) ;
#10534 = EDGE_CURVE ( 'NONE', #5330, #18127, #7489, .T. ) ;
#10535 = EDGE_LOOP ( 'NONE', ( #14458, #1351, #7448, #11401 ) ) ;
#10536 = DIRECTION ( 'NONE',  ( 0.000000000000000000, 0.5000000000000009992, 0.8660254037844381525 ) ) ;
#10537 = DIRECTION ( 'NONE',  ( 0.000000000000000000, 0.000000000000000000, 1.000000000000000000 ) ) ;
#10538 = ORIENTED_EDGE ( 'NONE', *, *, #4038, .T. ) ;
#10539 = AXIS2_PLACEMENT_3D ( 'NONE', #14772, #17663, #1966 ) ;
#10540 = VECTOR ( 'NONE', #17824, 1000.000000000000000 ) ;
#10541 = APPLICATION_PROTOCOL_DEFINITION ( 'draft international standard', 'automotive_design', 1998, #6188 ) ;
#10542 = DIRECTION ( 'NONE',  ( -0.9396926207859084279, 0.3420201433256686574, 0.000000000000000000 ) ) ;
#10543 =( NAMED_UNIT ( * ) PLANE_ANGLE_UNIT ( ) SI_UNIT ( $, .RADIAN. ) );
#10544 = AXIS2_PLACEMENT_3D ( 'NONE', #10442, #4645, #179 ) ;
#10545 = LINE ( 'NONE', #183, #5463 ) ;
#10546 = LINE ( 'NONE', #6218, #17164 ) ;
#10547 = VERTEX_POINT ( 'NONE', #7227 ) ;
#10548 = CARTESIAN_POINT ( 'NONE',  ( -107.5676225674731938, 110.5691553257988460, -22.35917033480641081 ) ) ;
#10549 = LINE ( 'NONE', #2122, #182 ) ;
#10550 = LINE ( 'NONE', #17644, #1378 ) ;
#10551 = DIRECTION ( 'NONE',  ( 0.000000000000000000, 0.000000000000000000, 1.000000000000000000 ) ) ;
#10552 = DIRECTION ( 'NONE',  ( 0.000000000000000000, 0.000000000000000000, 1.000000000000000000 ) ) ;
#10553 = ORIENTED_EDGE ( 'NONE', *, *, #17960, .F. ) ;
#10554 = VECTOR ( 'NONE', #2391, 1000.000000000000000 ) ;
#10555 = DIRECTION ( 'NONE',  ( 0.9396926207859185309, 0.3420201433256406798, -1.086737899653001478E-16 ) ) ;
#10556 = DIRECTION ( 'NONE',  ( 0.000000000000000000, 0.000000000000000000, 1.000000000000000000 ) ) ;
#10557 = ADVANCED_FACE ( 'NONE', ( #16004 ), #17307, .T. ) ;
#10558 = ORIENTED_EDGE ( 'NONE', *, *, #1963, .F. ) ;
#10559 = CARTESIAN_POINT ( 'NONE',  ( -92.59262256747321373, 117.8748711238780515, 25.00000000000000000 ) ) ;
#10560 = VECTOR ( 'NONE', #9630, 1000.000000000000114 ) ;
#10561 = VERTEX_POINT ( 'NONE', #4674 ) ;
#10562 = VECTOR ( 'NONE', #13891, 1000.000000000000000 ) ;
#10563 = ORIENTED_EDGE ( 'NONE', *, *, #7346, .T. ) ;
#10564 = DIRECTION ( 'NONE',  ( -0.000000000000000000, 0.000000000000000000, -1.000000000000000000 ) ) ;
#10565 = ORIENTED_EDGE ( 'NONE', *, *, #17478, .F. ) ;
#10566 = DIRECTION ( 'NONE',  ( -1.000000000000000000, -0.000000000000000000, -0.000000000000000000 ) ) ;
#10567 = DIRECTION ( 'NONE',  ( 0.9396926207859084279, 0.3420201433256686574, 0.000000000000000000 ) ) ;
#10568 = CARTESIAN_POINT ( 'NONE',  ( -72.32324610293285616, 109.3399659331339677, 22.53855496370561440 ) ) ;
#10569 = CARTESIAN_POINT ( 'NONE',  ( -25.66933353722515676, -111.0842361345572158, 5.654315315325685987 ) ) ;
#10570 = CIRCLE ( 'NONE', #13564, 11.04359719766049430 ) ;
#10571 = DIRECTION ( 'NONE',  ( 0.9396926207859078728, 0.3420201433256701007, 4.890320548438446933E-16 ) ) ;
#10572 = VECTOR ( 'NONE', #14880, 1000.000000000000000 ) ;
#10573 = DIRECTION ( 'NONE',  ( 0.000000000000000000, 0.000000000000000000, 1.000000000000000000 ) ) ;
#10574 = PRODUCT ( 'hex bolt gradeab fine_iso_ISO 8765 - M8x1.0 x 40 x 22-N', 'hex bolt gradeab fine_iso_ISO 8765 - M8x1.0 x 40 x 22-N', '', ( #6681 ) ) ;
#10575 = ORIENTED_EDGE ( 'NONE', *, *, #2983, .T. ) ;
#10576 = DIRECTION ( 'NONE',  ( -0.9396926207859084279, 0.3420201433256686574, -4.890320548438448905E-16 ) ) ;
#10577 = EDGE_CURVE ( 'NONE', #10198, #3816, #9974, .T. ) ;
#10578 = CARTESIAN_POINT ( 'NONE',  ( -76.14195937732675645, 61.88640485328121343, -26.51881048504861482 ) ) ;
#10579 = CARTESIAN_POINT ( 'NONE',  ( -67.59262256747317110, 57.88796029049329661, -30.35917033480639660 ) ) ;
#10580 = ORIENTED_EDGE ( 'NONE', *, *, #15206, .T. ) ;
#10581=STYLED_ITEM('',(#18566),#84);
#10582 = PLANE ( 'NONE',  #2853 ) ;
#10583 = DIRECTION ( 'NONE',  ( 0.000000000000000000, 0.000000000000000000, 1.000000000000000000 ) ) ;
#10584 = ORIENTED_EDGE ( 'NONE', *, *, #15902, .T. ) ;
#10585 = VECTOR ( 'NONE', #3880, 1000.000000000000000 ) ;
#10586 = CIRCLE ( 'NONE', #5799, 5.654315315325680658 ) ;
#10587 = AXIS2_PLACEMENT_3D ( 'NONE', #16593, #601, #3583 ) ;
#10588 = CIRCLE ( 'NONE', #9402, 180.8515291679561585 ) ;
#10589 = ORIENTED_EDGE ( 'NONE', *, *, #17940, .T. ) ;
#10590 = CARTESIAN_POINT ( 'NONE',  ( -57.08002265617300708, 84.22855780814606419, -167.1454815528550739 ) ) ;
#10591 = DIRECTION ( 'NONE',  ( 1.000000000000000000, 0.000000000000000000, 5.077734830647299712E-16 ) ) ;
#10592 = DIRECTION ( 'NONE',  ( 0.000000000000000000, 0.000000000000000000, 1.000000000000000000 ) ) ;
#10593 = EDGE_CURVE ( 'NONE', #11848, #15321, #12042, .T. ) ;
#10594 = PLANE ( 'NONE',  #3967 ) ;
#10595 =( GEOMETRIC_REPRESENTATION_CONTEXT ( 3 ) GLOBAL_UNCERTAINTY_ASSIGNED_CONTEXT ( ( #851 ) ) GLOBAL_UNIT_ASSIGNED_CONTEXT ( ( #7064, #5553, #11074 ) ) REPRESENTATION_CONTEXT ( 'NONE', 'WORKASPACE' ) );
#10596 = ORIENTED_EDGE ( 'NONE', *, *, #15319, .F. ) ;
#10597 = DIRECTION ( 'NONE',  ( 1.000000000000000000, 0.000000000000000000, 3.771137991253928573E-16 ) ) ;
#10598 = DIRECTION ( 'NONE',  ( 0.9396926207859065405, 0.3420201433256737089, 4.890320548438440031E-16 ) ) ;
#10599 = ORIENTED_EDGE ( 'NONE', *, *, #17045, .T. ) ;
#10600 = VECTOR ( 'NONE', #14643, 1000.000000000000000 ) ;
#10601 = DIRECTION ( 'NONE',  ( -1.000000000000000000, 0.000000000000000000, 0.000000000000000000 ) ) ;
#10602 = CARTESIAN_POINT ( 'NONE',  ( -66.00585202009862940, 110.5691553257988460, 25.00000000000000355 ) ) ;
#10603 = LINE ( 'NONE', #11904, #11501 ) ;
#10604 = CARTESIAN_POINT ( 'NONE',  ( -109.6936274348540508, -91.08423613455721579, 10.65431531532540177 ) ) ;
#10605 = EDGE_LOOP ( 'NONE', ( #3492, #14897, #7977, #7148 ) ) ;
#10606 = CIRCLE ( 'NONE', #11204, 26.04359719766049608 ) ;
#10607 = DIRECTION ( 'NONE',  ( 1.000000000000000000, 0.000000000000000000, 5.551115123125777772E-16 ) ) ;
#10608 = ORIENTED_EDGE ( 'NONE', *, *, #14853, .F. ) ;
#10609 = DIRECTION ( 'NONE',  ( 0.000000000000000000, 0.000000000000000000, 1.000000000000000000 ) ) ;
#10610 = ORIENTED_EDGE ( 'NONE', *, *, #4603, .T. ) ;
#10611 = VERTEX_POINT ( 'NONE', #3271 ) ;
#10612 = CIRCLE ( 'NONE', #17190, 5.654315315325682434 ) ;
#10613 = CIRCLE ( 'NONE', #4931, 42.49926016644946003 ) ;
#10614 = AXIS2_PLACEMENT_3D ( 'NONE', #9323, #6500, #15019 ) ;
#10615 = DIRECTION ( 'NONE',  ( 1.000000000000000000, 0.000000000000000000, 0.000000000000000000 ) ) ;
#10616 = CARTESIAN_POINT ( 'NONE',  ( -63.34052343625892689, 73.40930968350525632, -167.1454815528550739 ) ) ;
#10617 = ORIENTED_EDGE ( 'NONE', *, *, #18455, .T. ) ;
#10618 = EDGE_CURVE ( 'NONE', #8277, #1119, #11541, .T. ) ;
#10619 = LINE ( 'NONE', #9210, #8091 ) ;
#10620 = DIRECTION ( 'NONE',  ( 0.000000000000000000, 0.000000000000000000, -1.000000000000000000 ) ) ;
#10621 = VERTEX_POINT ( 'NONE', #14430 ) ;
#10622 = CARTESIAN_POINT ( 'NONE',  ( -68.99615306438111872, 8.293196988130274505, -167.1454815528550739 ) ) ;
#10623 = ORIENTED_EDGE ( 'NONE', *, *, #17697, .T. ) ;
#10624 = CARTESIAN_POINT ( 'NONE',  ( -57.89103256796045116, 73.45256821284057480, -167.1454815528550739 ) ) ;
#10625 = ORIENTED_EDGE ( 'NONE', *, *, #14423, .T. ) ;
#10626 = EDGE_CURVE ( 'NONE', #4697, #5159, #1609, .T. ) ;
#10627 = AXIS2_PLACEMENT_3D ( 'NONE', #12152, #17839, #2224 ) ;
#10628 = VECTOR ( 'NONE', #14748, 1000.000000000000000 ) ;
#10629 = DIRECTION ( 'NONE',  ( -0.000000000000000000, -0.000000000000000000, 1.000000000000000000 ) ) ;
#10630 = EDGE_CURVE ( 'NONE', #9602, #11331, #14443, .T. ) ;
#10631 = CARTESIAN_POINT ( 'NONE',  ( -81.37409655828226107, -91.08423613455721579, -38.97384619189710975 ) ) ;
#10632 = VERTEX_POINT ( 'NONE', #14517 ) ;
#10633 = ORIENTED_EDGE ( 'NONE', *, *, #7344, .F. ) ;
#10634 = EDGE_CURVE ( 'NONE', #13457, #2374, #13115, .T. ) ;
#10635 = VERTEX_POINT ( 'NONE', #5136 ) ;
#10636 = ADVANCED_FACE ( 'NONE', ( #17573 ), #4755, .F. ) ;
#10637 = DIRECTION ( 'NONE',  ( 0.000000000000000000, 1.000000000000000000, 0.000000000000000000 ) ) ;
#10638 = DIRECTION ( 'NONE',  ( 0.9396926207859185309, 0.3420201433256406798, 0.000000000000000000 ) ) ;
#10639 = ADVANCED_FACE ( 'NONE', ( #16450 ), #17951, .F. ) ;
#10640 = ORIENTED_EDGE ( 'NONE', *, *, #11657, .F. ) ;
#10641 = CARTESIAN_POINT ( 'NONE',  ( -71.24615306438079188, 113.6735582045637045, -167.1454815528550739 ) ) ;
#10642 = CARTESIAN_POINT ( 'NONE',  ( -68.99615306438104767, 36.56753083813026706, -15.00000000000001421 ) ) ;
#10643 = CYLINDRICAL_SURFACE ( 'NONE', #13865, 12.50000000000001066 ) ;
#10644 = ORIENTED_EDGE ( 'NONE', *, *, #17047, .F. ) ;
#10645 = CARTESIAN_POINT ( 'NONE',  ( -102.4618227840623774, -111.0842361345572158, -36.00000000000000000 ) ) ;
#10646 = FACE_OUTER_BOUND ( 'NONE', #16229, .T. ) ;
#10647 = LINE ( 'NONE', #909, #4249 ) ;
#10648 = ORIENTED_EDGE ( 'NONE', *, *, #1140, .T. ) ;
#10649 = ADVANCED_FACE ( 'NONE', ( #11973 ), #17409, .T. ) ;
#10650 = EDGE_CURVE ( 'NONE', #3501, #18444, #9356, .T. ) ;
#10651 = EDGE_CURVE ( 'NONE', #889, #6914, #15055, .T. ) ;
#10652 = DIRECTION ( 'NONE',  ( 0.000000000000000000, 6.938893903907234689E-15, 1.000000000000000000 ) ) ;
#10653 = CARTESIAN_POINT ( 'NONE',  ( -61.89532410461230683, -91.42293623445493722, 41.30285466933285221 ) ) ;
#10654 = VERTEX_POINT ( 'NONE', #12258 ) ;
#10655 = EDGE_CURVE ( 'NONE', #3274, #6455, #9451, .T. ) ;
#10656 = DIRECTION ( 'NONE',  ( 0.000000000000000000, 1.000000000000000000, 0.000000000000000000 ) ) ;
#10657 = LINE ( 'NONE', #1764, #612 ) ;
#10658 = EDGE_LOOP ( 'NONE', ( #9769, #3571 ) ) ;
#10659 = EDGE_LOOP ( 'NONE', ( #14138, #18278, #17509, #8310, #16101 ) ) ;
#10660 = EDGE_CURVE ( 'NONE', #1119, #3000, #9180, .T. ) ;
#10661 = CARTESIAN_POINT ( 'NONE',  ( -115.7702289486887395, -96.08423613455721579, -5.654315315326000402 ) ) ;
#10662 = ORIENTED_EDGE ( 'NONE', *, *, #2874, .T. ) ;
#10663 = EDGE_CURVE ( 'NONE', #5685, #15472, #9087, .T. ) ;
#10664 = DIRECTION ( 'NONE',  ( -1.047634945911800068E-14, 0.000000000000000000, 1.000000000000000000 ) ) ;
#10665 = CARTESIAN_POINT ( 'NONE',  ( -97.59262256747318531, 57.88796029049330372, 26.35917033480641436 ) ) ;
#10666 = EDGE_CURVE ( 'NONE', #8044, #15152, #3747, .T. ) ;
#10667 = CARTESIAN_POINT ( 'NONE',  ( -73.62694592582826658, 108.4942417827056289, 22.93390062366417936 ) ) ;
#10668 = CARTESIAN_POINT ( 'NONE',  ( -207.6107609645051753, 84.22855780814606419, 62.50000000000001421 ) ) ;
#10669 = CYLINDRICAL_SURFACE ( 'NONE', #7044, 12.49999999999999645 ) ;
#10670 = FACE_OUTER_BOUND ( 'NONE', #6416, .T. ) ;
#10671 = VERTEX_POINT ( 'NONE', #6159 ) ;
#10672 = DIRECTION ( 'NONE',  ( -0.000000000000000000, -0.000000000000000000, -1.000000000000000000 ) ) ;
#10673 = DIRECTION ( 'NONE',  ( 0.3420201433256661594, 0.9396926207859093161, -0.000000000000000000 ) ) ;
#10674 = ORIENTED_EDGE ( 'NONE', *, *, #13221, .T. ) ;
#10675 = DIRECTION ( 'NONE',  ( 0.000000000000000000, 1.000000000000000000, 0.000000000000000000 ) ) ;
#10676 = ORIENTED_EDGE ( 'NONE', *, *, #11577, .T. ) ;
#10677 = ORIENTED_EDGE ( 'NONE', *, *, #8239, .F. ) ;
#10678 = CARTESIAN_POINT ( 'NONE',  ( -57.08002265617300708, 84.22855780814606419, -15.00000000000001421 ) ) ;
#10679 = DIRECTION ( 'NONE',  ( 0.000000000000000000, 0.000000000000000000, 1.000000000000000000 ) ) ;
#10680 = CARTESIAN_POINT ( 'NONE',  ( -107.5926225674731853, 110.5691553257988460, 26.35917033480641436 ) ) ;
#10681 = DIRECTION ( 'NONE',  ( -0.9396926207859084279, 0.3420201433256686574, 0.000000000000000000 ) ) ;
#10682 = ORIENTED_EDGE ( 'NONE', *, *, #1271, .T. ) ;
#10683 = LINE ( 'NONE', #10774, #9248 ) ;
#10684 = ORIENTED_EDGE ( 'NONE', *, *, #16942, .T. ) ;
#10685 = CARTESIAN_POINT ( 'NONE',  ( -76.37409655828236055, -91.08423613455721579, -28.18308811886544873 ) ) ;
#10686 = LINE ( 'NONE', #17593, #3628 ) ;
#10687 = DIRECTION ( 'NONE',  ( -0.9396926207859022107, 0.3420201433256853663, 0.000000000000000000 ) ) ;
#10688 = CARTESIAN_POINT ( 'NONE',  ( -110.5389732269435115, -91.12516209206941653, 10.00231928999164133 ) ) ;
#10689 = EDGE_LOOP ( 'NONE', ( #9734, #5996, #10272, #2487 ) ) ;
#10690 = CARTESIAN_POINT ( 'NONE',  ( -66.27751174112272281, 84.22855780814606419, 92.50000000000000000 ) ) ;
#10691 = VERTEX_POINT ( 'NONE', #11881 ) ;
#10692 = CARTESIAN_POINT ( 'NONE',  ( -38.09490121289055509, 73.26749283227019305, 97.49999999999998579 ) ) ;
#10693 = ORIENTED_EDGE ( 'NONE', *, *, #16155, .F. ) ;
#10694 = EDGE_CURVE ( 'NONE', #14649, #18482, #18452, .T. ) ;
#10695 = VERTEX_POINT ( 'NONE', #12547 ) ;
#10696 = ADVANCED_FACE ( 'NONE', ( #16637 ), #11750, .T. ) ;
#10697 = SURFACE_SIDE_STYLE ('',( #9395 ) ) ;
#10698 = AXIS2_PLACEMENT_3D ( 'NONE', #1252, #12680, #15170 ) ;
#10699 = FACE_OUTER_BOUND ( 'NONE', #8472, .T. ) ;
#10700 = VERTEX_POINT ( 'NONE', #10954 ) ;
#10701 = DIRECTION ( 'NONE',  ( -1.000000000000000000, 0.000000000000000000, 1.692578276882434470E-16 ) ) ;
#10702 = CARTESIAN_POINT ( 'NONE',  ( -100.4870060002411805, -151.5628872026273086, 18.23991632971911869 ) ) ;
#10703 = ORIENTED_EDGE ( 'NONE', *, *, #226, .T. ) ;
#10704 = LINE ( 'NONE', #9306, #9002 ) ;
#10705 = EDGE_LOOP ( 'NONE', ( #9472, #3752, #16875, #10953 ) ) ;
#10706 = LINE ( 'NONE', #16399, #15604 ) ;
#10707 = FACE_OUTER_BOUND ( 'NONE', #14714, .T. ) ;
#10708 = CARTESIAN_POINT ( 'NONE',  ( -71.24615306438104767, 35.13374195456378857, -15.00000000000001421 ) ) ;
#10709 = VECTOR ( 'NONE', #17215, 1000.000000000000000 ) ;
#10710 = LINE ( 'NONE', #5194, #2076 ) ;
#10711 = ORIENTED_EDGE ( 'NONE', *, *, #18190, .T. ) ;
#10712 = VERTEX_POINT ( 'NONE', #3831 ) ;
#10713 = VERTEX_POINT ( 'NONE', #3926 ) ;
#10714 = DIRECTION ( 'NONE',  ( 1.000000000000000000, 0.000000000000000000, 3.771137991253923150E-16 ) ) ;
#10715 = CARTESIAN_POINT ( 'NONE',  ( -107.5926225674731853, 50.58224449241411236, 25.00000000000000000 ) ) ;
#10716 = ORIENTED_EDGE ( 'NONE', *, *, #2, .F. ) ;
#10717 = ADVANCED_FACE ( 'NONE', ( #13850 ), #15344, .T. ) ;
#10718 = CARTESIAN_POINT ( 'NONE',  ( -68.99615306438117557, 2.010011688130281193, -167.1454815528550739 ) ) ;
#10719 = CARTESIAN_POINT ( 'NONE',  ( -77.78732798123100167, 80.45864980048332882, 69.00206661717221834 ) ) ;
#10720 = CARTESIAN_POINT ( 'NONE',  ( -64.75543355702687620, 94.09456345901884333, -167.1454815528550739 ) ) ;
#10721 = VECTOR ( 'NONE', #10115, 1000.000000000000000 ) ;
#10722 = CYLINDRICAL_SURFACE ( 'NONE', #719, 12.50000000000001066 ) ;
#10723 = VERTEX_POINT ( 'NONE', #8138 ) ;
#10724 = LINE ( 'NONE', #16243, #16738 ) ;
#10725 = CARTESIAN_POINT ( 'NONE',  ( -46.95762973216378811, 85.83453492254348305, -15.00000000000001421 ) ) ;
#10726 = DIRECTION ( 'NONE',  ( 1.000000000000000000, 0.000000000000000000, 0.000000000000000000 ) ) ;
#10727 = FACE_OUTER_BOUND ( 'NONE', #8842, .T. ) ;
#10728 = ORIENTED_EDGE ( 'NONE', *, *, #3376, .F. ) ;
#10729 = CARTESIAN_POINT ( 'NONE',  ( 105.4583593777967963, -32.62665103886256190, -7.000000000000010658 ) ) ;
#10730 = CARTESIAN_POINT ( 'NONE',  ( -71.24615306438079188, 116.8151508545637114, -15.00000000000001421 ) ) ;
#10731 = EDGE_CURVE ( 'NONE', #14319, #9948, #7569, .T. ) ;
#10732 = ORIENTED_EDGE ( 'NONE', *, *, #10085, .F. ) ;
#10733 = ADVANCED_FACE ( 'NONE', ( #8240 ), #12361, .T. ) ;
#10734 = FACE_OUTER_BOUND ( 'NONE', #1434, .T. ) ;
#10735 = ORIENTED_EDGE ( 'NONE', *, *, #9022, .T. ) ;
#10736 = VECTOR ( 'NONE', #2086, 1000.000000000000114 ) ;
#10737 = ORIENTED_EDGE ( 'NONE', *, *, #16354, .T. ) ;
#10738 = VECTOR ( 'NONE', #1648, 1000.000000000000000 ) ;
#10739 =( REPRESENTATION_RELATIONSHIP ('NONE','NONE', #359, #14258 ) REPRESENTATION_RELATIONSHIP_WITH_TRANSFORMATION ( #18388 )SHAPE_REPRESENTATION_RELATIONSHIP( ) );
#10740 = CARTESIAN_POINT ( 'NONE',  ( -68.99615306438072082, 133.3420471316626958, 15.00000000000006928 ) ) ;
#10741 = EDGE_CURVE ( 'NONE', #415, #9366, #11459, .T. ) ;
#10742 = ORIENTED_EDGE ( 'NONE', *, *, #4566, .T. ) ;
#10743 = EDGE_CURVE ( 'NONE', #11134, #16609, #1880, .T. ) ;
#10744 = DIRECTION ( 'NONE',  ( 1.000000000000000000, 0.000000000000000000, 3.771137991253934490E-16 ) ) ;
#10745 = CARTESIAN_POINT ( 'NONE',  ( -71.20513298132846103, 58.47161403914679312, 22.38837701002785607 ) ) ;
#10746 = CARTESIAN_POINT ( 'NONE',  ( -68.05062368187118693, 78.23723799236674381, -167.1454815528550739 ) ) ;
#10747 = CARTESIAN_POINT ( 'NONE',  ( -49.93060289285580922, 91.57211267264388255, -15.00000000000001421 ) ) ;
#10748 = DIRECTION ( 'NONE',  ( -0.000000000000000000, -0.000000000000000000, 1.000000000000000000 ) ) ;
#10749 = PLANE ( 'NONE',  #14117 ) ;
#10750 = ORIENTED_EDGE ( 'NONE', *, *, #13373, .F. ) ;
#10751 = VECTOR ( 'NONE', #18374, 1000.000000000000000 ) ;
#10752 = EDGE_CURVE ( 'NONE', #5168, #14197, #723, .T. ) ;
#10753 = DIRECTION ( 'NONE',  ( 0.000000000000000000, 0.000000000000000000, -1.000000000000000000 ) ) ;
#10754 = VECTOR ( 'NONE', #11594, 1000.000000000000000 ) ;
#10755 = DIRECTION ( 'NONE',  ( -0.000000000000000000, -0.000000000000000000, 1.000000000000000000 ) ) ;
#10756 = EDGE_CURVE ( 'NONE', #16002, #12329, #8093, .T. ) ;
#10757 = ORIENTED_EDGE ( 'NONE', *, *, #13469, .F. ) ;
#10758 = CARTESIAN_POINT ( 'NONE',  ( -57.08002265617301418, 106.1506877598988154, 102.5000000000000000 ) ) ;
#10759 = DIRECTION ( 'NONE',  ( 0.000000000000000000, 1.000000000000000000, 0.000000000000000000 ) ) ;
#10760 = EDGE_CURVE ( 'NONE', #16099, #827, #6660, .T. ) ;
#10761 = ORIENTED_EDGE ( 'NONE', *, *, #17502, .F. ) ;
#10762 = EDGE_CURVE ( 'NONE', #7723, #13519, #9053, .T. ) ;
#10763 = MECHANICAL_DESIGN_GEOMETRIC_PRESENTATION_REPRESENTATION (  '', ( #14077 ), #12586 ) ;
#10764 = CIRCLE ( 'NONE', #10165, 12.49999999999999112 ) ;
#10765 = ORIENTED_EDGE ( 'NONE', *, *, #5509, .F. ) ;
#10766 = ADVANCED_FACE ( 'NONE', ( #2017 ), #5766, .F. ) ;
#10767 = AXIS2_PLACEMENT_3D ( 'NONE', #3072, #8879, #3246 ) ;
#10768 = AXIS2_PLACEMENT_3D ( 'NONE', #7208, #17121, #10108 ) ;
#10769 = DIRECTION ( 'NONE',  ( 0.000000000000000000, 0.000000000000000000, 1.000000000000000000 ) ) ;
#10770 = DIRECTION ( 'NONE',  ( -0.9396926207859097602, 0.3420201433256649937, 1.086737899652991371E-16 ) ) ;
#10771 = CARTESIAN_POINT ( 'NONE',  ( -42.22262702428728431, 53.23066522635949838, -25.06792223060221048 ) ) ;
#10772 = LINE ( 'NONE', #4768, #12036 ) ;
#10773 = ORIENTED_EDGE ( 'NONE', *, *, #15795, .F. ) ;
#10774 = CARTESIAN_POINT ( 'NONE',  ( -68.99615306438091977, 76.79337943166271430, -15.00000000000001421 ) ) ;
#10775 = PLANE ( 'NONE',  #4525 ) ;
#10776 = EDGE_LOOP ( 'NONE', ( #6102, #1552, #11272, #8295 ) ) ;
#10777 = DIRECTION ( 'NONE',  ( 0.000000000000000000, 5.551115123125747573E-17, 1.000000000000000000 ) ) ;
#10778 = CARTESIAN_POINT ( 'NONE',  ( 5.299999999999998934, -7.505553499465293932, 1.040834085586084257E-14 ) ) ;
#10779 = CARTESIAN_POINT ( 'NONE',  ( -57.08002265617300708, 84.22855780814606419, 7.000000000000009770 ) ) ;
#10780 = AXIS2_PLACEMENT_3D ( 'NONE', #2582, #15102, #5359 ) ;
#10781 = CARTESIAN_POINT ( 'NONE',  ( -114.6525958062276231, -93.09900722835551790, 6.628862765693201098 ) ) ;
#10782 = ORIENTED_EDGE ( 'NONE', *, *, #10398, .T. ) ;
#10783 = DIRECTION ( 'NONE',  ( 1.000000000000000000, -0.000000000000000000, -0.000000000000000000 ) ) ;
#10784 = ORIENTED_EDGE ( 'NONE', *, *, #10078, .F. ) ;
#10785 = AXIS2_PLACEMENT_3D ( 'NONE', #17810, #14818, #4990 ) ;
#10786 = VECTOR ( 'NONE', #7362, 1000.000000000000000 ) ;
#10787 = CARTESIAN_POINT ( 'NONE',  ( -107.5926225674731711, 57.88796029049330372, -26.35917033480641436 ) ) ;
#10788 = ORIENTED_EDGE ( 'NONE', *, *, #2999, .F. ) ;
#10789 = ORIENTED_EDGE ( 'NONE', *, *, #11202, .F. ) ;
#10790 = VECTOR ( 'NONE', #7152, 1000.000000000000000 ) ;
#10791 = CARTESIAN_POINT ( 'NONE',  ( -70.71978124295708312, -91.08423613455721579, 22.52877280353970235 ) ) ;
#10792 = CARTESIAN_POINT ( 'NONE',  ( -107.5676225674731654, 57.88796029049330372, 30.35917033480641081 ) ) ;
#10793 = FACE_OUTER_BOUND ( 'NONE', #5438, .T. ) ;
#10794 = VERTEX_POINT ( 'NONE', #15015 ) ;
#10795 = VECTOR ( 'NONE', #2347, 999.9999999999998863 ) ;
#10796 = VECTOR ( 'NONE', #11647, 1000.000000000000000 ) ;
#10797 = CARTESIAN_POINT ( 'NONE',  ( -68.99615306438083451, 96.25779118813026969, -167.1454815528550739 ) ) ;
#10798 = LINE ( 'NONE', #10904, #17753 ) ;
#10799 = ORIENTED_EDGE ( 'NONE', *, *, #13710, .F. ) ;
#10800 = CARTESIAN_POINT ( 'NONE',  ( -107.5676225674731654, 57.88796029049330372, -30.35917033480641081 ) ) ;
#10801 = CARTESIAN_POINT ( 'NONE',  ( -68.99615306438067819, 142.7668250816626596, -15.00000000000001421 ) ) ;
#10802 = EDGE_CURVE ( 'NONE', #14319, #12661, #13434, .T. ) ;
#10803 = ORIENTED_EDGE ( 'NONE', *, *, #13606, .F. ) ;
#10804 = DIRECTION ( 'NONE',  ( 1.000000000000000000, 0.000000000000000000, 0.000000000000000000 ) ) ;
#10805 = DIRECTION ( 'NONE',  ( 0.000000000000000000, 0.000000000000000000, 1.000000000000000000 ) ) ;
#10806 = AXIS2_PLACEMENT_3D ( 'NONE', #114, #16, #11613 ) ;
#10807 = DIRECTION ( 'NONE',  ( 1.000000000000000000, 0.000000000000000000, 5.551115123125777772E-16 ) ) ;
#10808 = LINE ( 'NONE', #3793, #16739 ) ;
#10809 = AXIS2_PLACEMENT_3D ( 'NONE', #11308, #12725, #18421 ) ;
#10810 = AXIS2_PLACEMENT_3D ( 'NONE', #16293, #676, #4771 ) ;
#10811 = ORIENTED_EDGE ( 'NONE', *, *, #14930, .F. ) ;
#10812 = ORIENTED_EDGE ( 'NONE', *, *, #7251, .T. ) ;
#10813 = PLANE ( 'NONE',  #11761 ) ;
#10814 = DIRECTION ( 'NONE',  ( 0.000000000000000000, 0.000000000000000000, -1.000000000000000000 ) ) ;
#10815 = VECTOR ( 'NONE', #8670, 1000.000000000000000 ) ;
#10816 = ORIENTED_EDGE ( 'NONE', *, *, #539, .T. ) ;
#10817 = CARTESIAN_POINT ( 'NONE',  ( -77.62069601435324273, 79.65130292775347698, 68.44629942221835961 ) ) ;
#10818 = LINE ( 'NONE', #10642, #3370 ) ;
#10819 = CARTESIAN_POINT ( 'NONE',  ( -67.77554565888843285, 85.77305660501664875, -167.1454815528550739 ) ) ;
#10820 = ORIENTED_EDGE ( 'NONE', *, *, #7909, .T. ) ;
#10821 = EDGE_CURVE ( 'NONE', #18179, #1519, #894, .T. ) ;
#10822 = CARTESIAN_POINT ( 'NONE',  ( -48.43547250063686960, 78.72276507608465579, 15.00000000000009592 ) ) ;
#10823 = CIRCLE ( 'NONE', #3349, 10.24900000000000766 ) ;
#10824 = CIRCLE ( 'NONE', #3335, 3.999999999999989786 ) ;
#10825 = CARTESIAN_POINT ( 'NONE',  ( -56.41614838398844256, 95.01461175692088545, 15.00000000000006928 ) ) ;
#10826 = DIRECTION ( 'NONE',  ( 1.000000000000000000, 0.000000000000000000, 3.771137991253928573E-16 ) ) ;
#10827 = EDGE_LOOP ( 'NONE', ( #11049, #5029, #18160, #15687 ) ) ;
#10828 = CARTESIAN_POINT ( 'NONE',  ( -57.08002265617300708, 84.22855780814606419, 77.50000000000000000 ) ) ;
#10829 = CARTESIAN_POINT ( 'NONE',  ( -76.37409655828219002, -96.08423613455721579, -45.05044770573186952 ) ) ;
#10830 = ORIENTED_EDGE ( 'NONE', *, *, #3164, .F. ) ;
#10831 = VECTOR ( 'NONE', #9208, 1000.000000000000000 ) ;
#10832 = ADVANCED_FACE ( 'NONE', ( #12039 ), #18014, .T. ) ;
#10833 = CARTESIAN_POINT ( 'NONE',  ( -71.24615306438091977, 71.94398301522919326, -15.00000000000001421 ) ) ;
#10834 = CARTESIAN_POINT ( 'NONE',  ( -36.37271733111500538, 80.45864980048332882, 55.99793338282779587 ) ) ;
#10835 = ORIENTED_EDGE ( 'NONE', *, *, #333, .T. ) ;
#10836 = ORIENTED_EDGE ( 'NONE', *, *, #4430, .F. ) ;
#10837 = AXIS2_PLACEMENT_3D ( 'NONE', #15816, #1598, #16071 ) ;
#10838 = VECTOR ( 'NONE', #2945, 1000.000000000000000 ) ;
#10839 = CARTESIAN_POINT ( 'NONE',  ( -48.43547250063686960, 78.72276507608465579, -15.00000000000001421 ) ) ;
#10840 = VERTEX_POINT ( 'NONE', #3712 ) ;
#10841 = DIRECTION ( 'NONE',  ( 1.156482317317869999E-16, 0.000000000000000000, 1.000000000000000000 ) ) ;
#10842 = CARTESIAN_POINT ( 'NONE',  ( -68.99615306438100504, 39.70912348813028103, -167.1454815528550739 ) ) ;
#10843 = CARTESIAN_POINT ( 'NONE',  ( -81.37409655828265898, -91.08423613455721579, -8.525034724645805924E-13 ) ) ;
#10844 = EDGE_CURVE ( 'NONE', #10849, #18394, #13712, .T. ) ;
#10845 = CARTESIAN_POINT ( 'NONE',  ( -71.24615306438097662, 56.23601976522923707, 15.00000000000006928 ) ) ;
#10846 = CARTESIAN_POINT ( 'NONE',  ( -58.51182448057780050, 96.64628479562776420, 15.00000000000006928 ) ) ;
#10847 = CARTESIAN_POINT ( 'NONE',  ( -92.59262256747319952, 57.88796029049330372, 30.35917033480640370 ) ) ;
#10848 = DIRECTION ( 'NONE',  ( 1.000000000000000000, 0.000000000000000000, 6.950654929607132427E-15 ) ) ;
#10849 = VERTEX_POINT ( 'NONE', #3422 ) ;
#10850 = CARTESIAN_POINT ( 'NONE',  ( -71.24615306438100504, 53.09442711522921599, -15.00000000000001421 ) ) ;
#10851 = VECTOR ( 'NONE', #5804, 1000.000000000000000 ) ;
#10852 = AXIS2_PLACEMENT_3D ( 'NONE', #8901, #5813, #17227 ) ;
#10853 = VECTOR ( 'NONE', #8782, 1000.000000000000000 ) ;
#10854 = DIRECTION ( 'NONE',  ( 0.000000000000000000, -0.000000000000000000, 1.000000000000000000 ) ) ;
#10855 = ORIENTED_EDGE ( 'NONE', *, *, #7357, .F. ) ;
#10856 = EDGE_CURVE ( 'NONE', #14316, #6278, #7269, .T. ) ;
#10857 = CARTESIAN_POINT ( 'NONE',  ( -27.30335599338096841, -92.58099833983887095, -7.070576347711321930 ) ) ;
#10858 = DIRECTION ( 'NONE',  ( 0.9396926207859069846, 0.3420201433256723766, -1.086737899652988166E-16 ) ) ;
#10859 = ORIENTED_EDGE ( 'NONE', *, *, #8600, .T. ) ;
#10860 = ORIENTED_EDGE ( 'NONE', *, *, #14075, .F. ) ;
#10861 = ORIENTED_EDGE ( 'NONE', *, *, #16346, .T. ) ;
#10862 = PRODUCT_DEFINITION_FORMATION_WITH_SPECIFIED_SOURCE ( 'ANY', '', #18381, .NOT_KNOWN. ) ;
#10863 = EDGE_CURVE ( 'NONE', #8038, #1895, #5472, .T. ) ;
#10864 = CIRCLE ( 'NONE', #15346, 29.36884788726140627 ) ;
#10865 = CARTESIAN_POINT ( 'NONE',  ( -194.4437806548868934, -111.0842361345572158, -18.23991632971910803 ) ) ;
#10866 = DIRECTION ( 'NONE',  ( -5.204170427930409450E-16, 0.000000000000000000, 1.000000000000000000 ) ) ;
#10867 = EDGE_CURVE ( 'NONE', #2786, #10840, #9071, .T. ) ;
#10868 = CARTESIAN_POINT ( 'NONE',  ( -70.71978124295696944, -141.5628872026273086, -18.23991632971910803 ) ) ;
#10869 = DIRECTION ( 'NONE',  ( -0.000000000000000000, 0.000000000000000000, 1.000000000000000000 ) ) ;
#10870 = EDGE_CURVE ( 'NONE', #14275, #5132, #11937, .T. ) ;
#10871 = DIRECTION ( 'NONE',  ( 0.000000000000000000, 0.000000000000000000, 1.000000000000000000 ) ) ;
#10872 = CARTESIAN_POINT ( 'NONE',  ( -107.5926225674732137, 107.8748711238780373, 35.00000000000000000 ) ) ;
#10873 = ADVANCED_FACE ( 'NONE', ( #14829 ), #620, .F. ) ;
#10874 = ORIENTED_EDGE ( 'NONE', *, *, #14412, .T. ) ;
#10875 = DIRECTION ( 'NONE',  ( -0.000000000000000000, -1.000000000000000000, -0.000000000000000000 ) ) ;
#10876 = CARTESIAN_POINT ( 'NONE',  ( -71.24615306438070661, 141.9478920545637664, -167.1454815528550739 ) ) ;
#10878 = ORIENTED_EDGE ( 'NONE', *, *, #1563, .F. ) ;
#10877 = CARTESIAN_POINT ( 'NONE',  ( -78.12361985383350316, 84.22855780814606419, 55.00000000000001421 ) ) ;
#10879 = CARTESIAN_POINT ( 'NONE',  ( -110.3711597500469566, -91.10977358899566525, 10.13292356933293270 ) ) ;
#10880 = DIRECTION ( 'NONE',  ( -0.000000000000000000, 1.000000000000000000, -0.000000000000000000 ) ) ;
#10881 = ORIENTED_EDGE ( 'NONE', *, *, #7992, .F. ) ;
#10882 = B_SPLINE_CURVE_WITH_KNOTS ( 'NONE', 3,
 ( #6899, #1200, #4099, #5492, #12625, #9802, #7668, #4953, #10667, #11703, #10568, #17664, #378, #16164, #16352, #16271 ),
 .UNSPECIFIED., .F., .F.,
 ( 4, 2, 2, 2, 2, 2, 2, 4 ),
 ( 0.000000000000000000, 0.0009642797493039184610, 0.001928559498607836922, 0.002892839247911755708, 0.003857118997215673844, 0.005785678495823502743, 0.006749958245127435190, 0.007714237994431366770 ),
 .UNSPECIFIED. ) ;
#10883 = ADVANCED_FACE ( 'NONE', ( #16410 ), #5097, .T. ) ;
#10884 = EDGE_CURVE ( 'NONE', #4573, #677, #16323, .T. ) ;
#10885 = AXIS2_PLACEMENT_3D ( 'NONE', #10819, #3515, #10928 ) ;
#10886 = ADVANCED_FACE ( 'NONE', ( #13633 ), #808, .T. ) ;
#10887 = DIRECTION ( 'NONE',  ( 1.000000000000000000, 0.000000000000000000, 0.000000000000000000 ) ) ;
#10889 = ORIENTED_EDGE ( 'NONE', *, *, #14853, .T. ) ;
#10888 = VECTOR ( 'NONE', #16089, 1000.000000000000000 ) ;
#10890 = PRODUCT_DEFINITION_SHAPE ( 'NONE', 'NONE',  #13786 ) ;
#10891 = EDGE_CURVE ( 'NONE', #4298, #2330, #12795, .T. ) ;
#10892 = ORIENTED_EDGE ( 'NONE', *, *, #3995, .F. ) ;
#10893 = VECTOR ( 'NONE', #11178, 1000.000000000000000 ) ;
#10894 = DIRECTION ( 'NONE',  ( 0.000000000000000000, 0.000000000000000000, 1.000000000000000000 ) ) ;
#10895 = CARTESIAN_POINT ( 'NONE',  ( -65.72457281170906640, 78.72276507608454210, 15.00000000000006928 ) ) ;
#10896 = PLANE ( 'NONE',  #13803 ) ;
#10897 = ORIENTED_EDGE ( 'NONE', *, *, #14423, .F. ) ;
#10898 = ITEM_DEFINED_TRANSFORMATION ( 'NONE', 'NONE', #12682,  #16217 ) ;
#10899 = AXIS2_PLACEMENT_3D ( 'NONE', #7628, #13243, #11573 ) ;
#10900 = EDGE_CURVE ( 'NONE', #2011, #10849, #11174, .T. ) ;
#10901 = AXIS2_PLACEMENT_3D ( 'NONE', #5708, #14328, #7310 ) ;
#10902 = CARTESIAN_POINT ( 'NONE',  ( -98.90286936182235422, -91.08423613455721579, -2.027180301682503564E-13 ) ) ;
#10903 = EDGE_CURVE ( 'NONE', #9885, #16487, #9367, .T. ) ;
#10904 = CARTESIAN_POINT ( 'NONE',  ( -71.24615306438069240, 138.8062994045637311, -15.00000000000001421 ) ) ;
#10905 = VERTEX_POINT ( 'NONE', #16897 ) ;
#10906 = CARTESIAN_POINT ( 'NONE',  ( -57.08002265617300708, 84.22855780814606419, 15.00000000000006928 ) ) ;
#10907 = CARTESIAN_POINT ( 'NONE',  ( -71.24615306438109030, 28.85055665456373575, -167.1454815528550739 ) ) ;
#10908 = CARTESIAN_POINT ( 'NONE',  ( -62.11705611183893438, 93.78931001713317528, -167.1454815528550739 ) ) ;
#10909 = VERTEX_POINT ( 'NONE', #8490 ) ;
#10910 = CARTESIAN_POINT ( 'NONE',  ( -76.04905332431492582, 106.6498183473933068, -27.18785666068412610 ) ) ;
#10911 = CARTESIAN_POINT ( 'NONE',  ( -66.00585202009862940, 110.5691553257988460, 25.00000000000000355 ) ) ;
#10912 = ORIENTED_EDGE ( 'NONE', *, *, #7545, .F. ) ;
#10913 = CARTESIAN_POINT ( 'NONE',  ( -57.08002265617300708, 84.22855780814606419, 15.00000000000006928 ) ) ;
#10914 = VECTOR ( 'NONE', #15109, 1000.000000000000000 ) ;
#10915 = LINE ( 'NONE', #11931, #7745 ) ;
#10916 = AXIS2_PLACEMENT_3D ( 'NONE', #13748, #7950, #2242 ) ;
#10917 = ORIENTED_EDGE ( 'NONE', *, *, #3001, .T. ) ;
#10918 = VECTOR ( 'NONE', #16138, 1000.000000000000000 ) ;
#10919 = B_SPLINE_CURVE_WITH_KNOTS ( 'NONE', 3,
 ( #13188, #7468, #3253, #271, #11781, #7658, #14668, #367, #3175, #11954, #4568, #6230 ),
 .UNSPECIFIED., .F., .F.,
 ( 4, 2, 2, 2, 2, 4 ),
 ( 0.01258489339592914341, 0.01361446459519792193, 0.01464403579446670045, 0.01567360699373548244, 0.01618839259336985956, 0.01670317819300424014 ),
 .UNSPECIFIED. ) ;
#10920 = VERTEX_POINT ( 'NONE', #18493 ) ;
#10921 = DIRECTION ( 'NONE',  ( 0.000000000000000000, 1.000000000000000000, 0.000000000000000000 ) ) ;
#10922 = CARTESIAN_POINT ( 'NONE',  ( -68.99615306438104767, 30.28434553813026398, -15.00000000000001421 ) ) ;
#10923 = EDGE_CURVE ( 'NONE', #3472, #13404, #1905, .T. ) ;
#10924 = VERTEX_POINT ( 'NONE', #9701 ) ;
#10925 = LINE ( 'NONE', #9794, #17902 ) ;
#10926 = CARTESIAN_POINT ( 'NONE',  ( -76.83752720176745754, 76.98425793134822470, 64.45727744071827203 ) ) ;
#10927 = CARTESIAN_POINT ( 'NONE',  ( 105.4583593777967963, -32.62665103886256190, 7.000000000000010658 ) ) ;
#10928 = DIRECTION ( 'NONE',  ( 1.000000000000000000, 0.000000000000000000, 0.000000000000000000 ) ) ;
#10929 = VERTEX_POINT ( 'NONE', #5380 ) ;
#10930 = CARTESIAN_POINT ( 'NONE',  ( -67.20241558018224737, 85.83453492254335515, -15.00000000000001243 ) ) ;
#10931 = CARTESIAN_POINT ( 'NONE',  ( -71.24615306438103346, 46.81124181522922356, -15.00000000000001421 ) ) ;
#10932 = AXIS2_PLACEMENT_3D ( 'NONE', #12227, #8008, #3997 ) ;
#10933 = LINE ( 'NONE', #15421, #12008 ) ;
#10934 = CARTESIAN_POINT ( 'NONE',  ( -71.24615306438080609, 103.3599095152292193, -15.00000000000001421 ) ) ;
#10935 = ORIENTED_EDGE ( 'NONE', *, *, #16227, .F. ) ;
#10936 = CARTESIAN_POINT ( 'NONE',  ( 5.299999999999998934, 3.752776749732435135, 6.499999999999981348 ) ) ;
#10937 = DIRECTION ( 'NONE',  ( 1.000000000000000000, -0.000000000000000000, 1.047634945911799279E-14 ) ) ;
#10938 = VERTEX_POINT ( 'NONE', #5662 ) ;
#10939 = CARTESIAN_POINT ( 'NONE',  ( -68.99615306438080609, 105.6825691381303045, -167.1454815528550739 ) ) ;
#10940 = CARTESIAN_POINT ( 'NONE',  ( -36.30023241575587178, 80.89962780276930232, 69.22524214366039530 ) ) ;
#10941 = ORIENTED_EDGE ( 'NONE', *, *, #8936, .F. ) ;
#10942 = ADVANCED_FACE ( 'NONE', ( #5295 ), #16793, .T. ) ;
#10943 = VERTEX_POINT ( 'NONE', #2681 ) ;
#10944 = DIRECTION ( 'NONE',  ( 0.000000000000000000, 0.000000000000000000, 1.000000000000000000 ) ) ;
#10945 = EDGE_CURVE ( 'NONE', #18464, #5754, #17083, .T. ) ;
#10946 = ORIENTED_EDGE ( 'NONE', *, *, #11765, .T. ) ;
#10947 = LINE ( 'NONE', #11319, #1075 ) ;
#10948 = DIRECTION ( 'NONE',  ( 0.000000000000000000, 0.000000000000000000, 1.000000000000000000 ) ) ;
#10949 = CARTESIAN_POINT ( 'NONE',  ( -66.17295708481962890, 57.85212116841895380, -28.00000000000000355 ) ) ;
#10950 = CARTESIAN_POINT ( 'NONE',  ( -44.49764538373973721, 84.22855780814606419, 37.50000000000000000 ) ) ;
#10951 = DIRECTION ( 'NONE',  ( -1.000000000000000000, -2.062304371594500247E-16, 0.000000000000000000 ) ) ;
#10952 = FACE_OUTER_BOUND ( 'NONE', #17678, .T. ) ;
#10953 = ORIENTED_EDGE ( 'NONE', *, *, #14331, .F. ) ;
#10954 = CARTESIAN_POINT ( 'NONE',  ( -68.99615306438097662, 58.55867938813025830, 15.00000000000006928 ) ) ;
#10955 = PLANE ( 'NONE',  #15250 ) ;
#10956 = ORIENTED_EDGE ( 'NONE', *, *, #17950, .T. ) ;
#10957 = CARTESIAN_POINT ( 'NONE',  ( -30.90059672715241845, -91.12516132330414109, -10.00232511491633325 ) ) ;
#10958 = CARTESIAN_POINT ( 'NONE',  ( -57.08002265617300708, 84.22855780814606419, 77.50000000000000000 ) ) ;
#10959 = ORIENTED_EDGE ( 'NONE', *, *, #3791, .F. ) ;
#10960 = VERTEX_POINT ( 'NONE', #11010 ) ;
#10961 = ORIENTED_EDGE ( 'NONE', *, *, #3771, .F. ) ;
#10962 = PRODUCT_DEFINITION_CONTEXT ( 'detailed design', #12931, 'design' ) ;
#10963 = LINE ( 'NONE', #17029, #16556 ) ;
#10964 = CARTESIAN_POINT ( 'NONE',  ( -71.24615306438117557, 3.717815454563750954, -167.1454815528550739 ) ) ;
#10965 = FACE_OUTER_BOUND ( 'NONE', #11414, .T. ) ;
#10966 = CARTESIAN_POINT ( 'NONE',  ( -71.24615306438076345, 119.0678727652292253, 15.00000000000006928 ) ) ;
#10967 = EDGE_CURVE ( 'NONE', #425, #4999, #3886, .T. ) ;
#10968 = CARTESIAN_POINT ( 'NONE',  ( -49.97371631896665178, 107.0896764944441202, 97.49999999999998579 ) ) ;
#10969 = DIRECTION ( 'NONE',  ( -1.000000000000000000, -0.000000000000000000, -0.000000000000000000 ) ) ;
#10970 = ORIENTED_EDGE ( 'NONE', *, *, #10409, .T. ) ;
#10971 = CARTESIAN_POINT ( 'NONE',  ( 93.45071565215914688, 84.22855780814606419, 62.50000000000001421 ) ) ;
#10972 = DIRECTION ( 'NONE',  ( 0.000000000000000000, 0.000000000000000000, -1.000000000000000000 ) ) ;
#10974 = ORIENTED_EDGE ( 'NONE', *, *, #4814, .F. ) ;
#10973 = CARTESIAN_POINT ( 'NONE',  ( -78.10583027636772613, 85.21903647478332289, 69.95048561006090893 ) ) ;
#10975 = CARTESIAN_POINT ( 'NONE',  ( -68.99615306438086293, 89.35975003166268493, 15.00000000000006928 ) ) ;
#10976 = DIRECTION ( 'NONE',  ( 0.000000000000000000, 1.000000000000000000, -0.000000000000000000 ) ) ;
#10977 = EDGE_LOOP ( 'NONE', ( #8366, #2393, #18039, #14245 ) ) ;
#10978 = VERTEX_POINT ( 'NONE', #11105 ) ;
#10979 = ADVANCED_FACE ( 'NONE', ( #14199 ), #8391, .F. ) ;
#10980 = EDGE_CURVE ( 'NONE', #4127, #18127, #14006, .T. ) ;
#10981 = ORIENTED_EDGE ( 'NONE', *, *, #16926, .F. ) ;
#10982 = LINE ( 'NONE', #594, #9709 ) ;
#10983 = FACE_OUTER_BOUND ( 'NONE', #10061, .T. ) ;
#10984 = EDGE_CURVE ( 'NONE', #6666, #1661, #3988, .T. ) ;
#10985 = ORIENTED_EDGE ( 'NONE', *, *, #9034, .T. ) ;
#10986 = CONTEXT_DEPENDENT_SHAPE_REPRESENTATION ( #7876, #553 ) ;
#10987 = EDGE_CURVE ( 'NONE', #10700, #16781, #18120, .T. ) ;
#10988 = EDGE_CURVE ( 'NONE', #7322, #14963, #2820, .T. ) ;
#10989 = CARTESIAN_POINT ( 'NONE',  ( -31.06841040534018106, -91.10977296152353233, 10.13292952605207375 ) ) ;
#10990 = DIRECTION ( 'NONE',  ( 0.000000000000000000, 0.000000000000000000, -1.000000000000000000 ) ) ;
#10991 = VERTEX_POINT ( 'NONE', #8200 ) ;
#10992 = FACE_OUTER_BOUND ( 'NONE', #11580, .T. ) ;
#10993 = FACE_OUTER_BOUND ( 'NONE', #14898, .T. ) ;
#10994 = DIRECTION ( 'NONE',  ( 1.119176436114069332E-16, -1.000000000000000000, -0.000000000000000000 ) ) ;
#10995 = VERTEX_POINT ( 'NONE', #13915 ) ;
#10996 = CARTESIAN_POINT ( 'NONE',  ( -67.59262256747319952, 110.5691553257988460, 30.35917033480640370 ) ) ;
#10997 = DIRECTION ( 'NONE',  ( 0.000000000000000000, 0.000000000000000000, 1.000000000000000000 ) ) ;
#10998 = ORIENTED_EDGE ( 'NONE', *, *, #3456, .F. ) ;
#10999 = EDGE_CURVE ( 'NONE', #9582, #850, #12375, .T. ) ;
#11000 = CARTESIAN_POINT ( 'NONE',  ( -57.08002265617300708, 84.22855780814606419, 15.00000000000006928 ) ) ;
#11001 = APPLICATION_CONTEXT ( 'automotive_design' ) ;
#11002 = CARTESIAN_POINT ( 'NONE',  ( -67.59262256747317110, 56.80567558672318995, -22.50837044127973030 ) ) ;
#11003 = ORIENTED_EDGE ( 'NONE', *, *, #4378, .F. ) ;
#11004 = ADVANCED_FACE ( 'NONE', ( #12516 ), #1287, .T. ) ;
#11005 = EDGE_CURVE ( 'NONE', #11474, #14401, #12713, .T. ) ;
#11006 = AXIS2_PLACEMENT_3D ( 'NONE', #15556, #12487, #4148 ) ;
#11007 = ORIENTED_EDGE ( 'NONE', *, *, #11233, .F. ) ;
#11008 = ORIENTED_EDGE ( 'NONE', *, *, #2524, .T. ) ;
#11009 = DIRECTION ( 'NONE',  ( 0.000000000000000000, 0.000000000000000000, 1.000000000000000000 ) ) ;
#11010 = CARTESIAN_POINT ( 'NONE',  ( -68.99615306438077766, 117.6340838816626899, -15.00000000000001421 ) ) ;
#11011 = ADVANCED_FACE ( 'NONE', ( #5480 ), #11207, .T. ) ;
#11012 = ORIENTED_EDGE ( 'NONE', *, *, #7900, .F. ) ;
#11013 = CYLINDRICAL_SURFACE ( 'NONE', #17053, 34.36884788726141693 ) ;
#11014 = LINE ( 'NONE', #14009, #11623 ) ;
#11015 = DIRECTION ( 'NONE',  ( -1.000000000000000000, 0.000000000000000000, 0.000000000000000000 ) ) ;
#11016 = DIRECTION ( 'NONE',  ( 1.000000000000000000, 2.062304371594500494E-16, 0.000000000000000000 ) ) ;
#11017 = EDGE_LOOP ( 'NONE', ( #7211, #14659, #17641, #8237 ) ) ;
#11018 = DIRECTION ( 'NONE',  ( 0.000000000000000000, -5.551115123125748806E-17, -1.000000000000000000 ) ) ;
#11019 = CARTESIAN_POINT ( 'NONE',  ( 93.45071565215914688, 84.22855780814606419, 62.50000000000001421 ) ) ;
#11020 = LINE ( 'NONE', #906, #2870 ) ;
#11021 = DIRECTION ( 'NONE',  ( 1.000000000000000000, 0.000000000000000000, 0.000000000000000000 ) ) ;
#11022 = CARTESIAN_POINT ( 'NONE',  ( -57.08002265617300708, 84.22855780814606419, -167.1454815528550739 ) ) ;
#11023 = VERTEX_POINT ( 'NONE', #16034 ) ;
#11024 = FACE_OUTER_BOUND ( 'NONE', #10776, .T. ) ;
#11025 = CARTESIAN_POINT ( 'NONE',  ( -61.10958520376166803, -91.18731141006419705, 40.31989393471906169 ) ) ;
#11026 = CARTESIAN_POINT ( 'NONE',  ( -97.59262256747319952, 57.88796029049330372, -26.35917033480641436 ) ) ;
#11027 = CARTESIAN_POINT ( 'NONE',  ( -37.24053394569259723, 77.21161119120516503, 59.84068429610289286 ) ) ;
#11028 = VERTEX_POINT ( 'NONE', #59 ) ;
#11029 = VERTEX_POINT ( 'NONE', #16112 ) ;
#11030 = CIRCLE ( 'NONE', #5657, 4.999999999999999112 ) ;
#11031 = CARTESIAN_POINT ( 'NONE',  ( 0.06682554136346589846, -6.264794173742427752, -2.149058192116912291 ) ) ;
#11032 = ORIENTED_EDGE ( 'NONE', *, *, #7251, .F. ) ;
#11033 = DIRECTION ( 'NONE',  ( 0.000000000000000000, 0.000000000000000000, 1.000000000000000000 ) ) ;
#11034 = CARTESIAN_POINT ( 'NONE',  ( 5.299999999999998934, 3.752776749732559924, -6.500000000000061284 ) ) ;
#11035 = CARTESIAN_POINT ( 'NONE',  ( -66.01768795098074349, 57.62469735380677349, 25.00000000000000355 ) ) ;
#11036 = CARTESIAN_POINT ( 'NONE',  ( -68.99615306438083451, 102.5409764881302692, 15.00000000000006928 ) ) ;
#11037 = CARTESIAN_POINT ( 'NONE',  ( -71.24615306438109030, 24.82009326522924297, 15.00000000000006928 ) ) ;
#11038 = FACE_OUTER_BOUND ( 'NONE', #17165, .T. ) ;
#11039 = CARTESIAN_POINT ( 'NONE',  ( -71.24615306438113294, 10.00100075456376025, -15.00000000000001421 ) ) ;
#11040 = PRODUCT_DEFINITION_SHAPE ( 'NONE', 'NONE',  #4980 ) ;
#11041 = ORIENTED_EDGE ( 'NONE', *, *, #548, .F. ) ;
#11042 = DIRECTION ( 'NONE',  ( 0.000000000000000000, 0.000000000000000000, -1.000000000000000000 ) ) ;
#11043 = FACE_OUTER_BOUND ( 'NONE', #2971, .T. ) ;
#11044 = AXIS2_PLACEMENT_3D ( 'NONE', #12599, #16974, #5286 ) ;
#11045 = ORIENTED_EDGE ( 'NONE', *, *, #17723, .F. ) ;
#11046 = CARTESIAN_POINT ( 'NONE',  ( -71.24615306438117557, 6.859408104563785358, -167.1454815528550739 ) ) ;
#11047 = VECTOR ( 'NONE', #6798, 1000.000000000000000 ) ;
#11048 = CARTESIAN_POINT ( 'NONE',  ( -69.26154997389620860, 57.49002305898234511, 22.35917033480642502 ) ) ;
#11049 = ORIENTED_EDGE ( 'NONE', *, *, #8004, .F. ) ;
#11050 = ORIENTED_EDGE ( 'NONE', *, *, #5959, .T. ) ;
#11051 = EDGE_LOOP ( 'NONE', ( #17841, #17101, #9334, #4826 ) ) ;
#11052 = PLANE ( 'NONE',  #17453 ) ;
#11053 = DIRECTION ( 'NONE',  ( 0.000000000000000000, 0.000000000000000000, 1.000000000000000000 ) ) ;
#11054 = CIRCLE ( 'NONE', #4476, 4.600000000000006750 ) ;
#11055 = DIRECTION ( 'NONE',  ( 1.156482317317869999E-16, 0.000000000000000000, 1.000000000000000000 ) ) ;
#11056 = DIRECTION ( 'NONE',  ( 1.000000000000000000, 0.000000000000000000, 0.000000000000000000 ) ) ;
#11057 = DIRECTION ( 'NONE',  ( 0.000000000000000000, 1.000000000000000000, 0.000000000000000000 ) ) ;
#11058 = VECTOR ( 'NONE', #1385, 1000.000000000000000 ) ;
#11059 = DIRECTION ( 'NONE',  ( 1.000000000000000000, 0.000000000000000000, 0.000000000000000000 ) ) ;
#11060 = FACE_OUTER_BOUND ( 'NONE', #15183, .T. ) ;
#11061 = ORIENTED_EDGE ( 'NONE', *, *, #14739, .F. ) ;
#11062 = CARTESIAN_POINT ( 'NONE',  ( -71.24615306438111872, 21.67850061522927518, -167.1454815528550739 ) ) ;
#11063 = LINE ( 'NONE', #1069, #4524 ) ;
#11065 = VERTEX_POINT ( 'NONE', #5756 ) ;
#11064 = CARTESIAN_POINT ( 'NONE',  ( -77.09753311995068259, 90.72064142110008333, 66.26335585294400232 ) ) ;
#11066 = DIRECTION ( 'NONE',  ( 0.000000000000000000, 0.000000000000000000, -1.000000000000000000 ) ) ;
#11067 = VERTEX_POINT ( 'NONE', #1647 ) ;
#11068 = CARTESIAN_POINT ( 'NONE',  ( -127.5926225674731995, 106.9211863004614997, -28.00000000000000355 ) ) ;
#11069 = ORIENTED_EDGE ( 'NONE', *, *, #3063, .F. ) ;
#11070 = VECTOR ( 'NONE', #5697, 1000.000000000000000 ) ;
#11071 = EDGE_CURVE ( 'NONE', #7151, #10506, #17524, .T. ) ;
#11072 = AXIS2_PLACEMENT_3D ( 'NONE', #14120, #11405, #15426 ) ;
#11073 = ORIENTED_EDGE ( 'NONE', *, *, #8953, .T. ) ;
#11074 =( NAMED_UNIT ( * ) SI_UNIT ( $, .STERADIAN. ) SOLID_ANGLE_UNIT ( ) );
#11075 = DIRECTION ( 'NONE',  ( 1.000000000000000000, 0.000000000000000000, 0.000000000000000000 ) ) ;
#11076 = CARTESIAN_POINT ( 'NONE',  ( -57.08002265617300708, 84.22855780814606419, 15.00000000000006928 ) ) ;
#11077 = ORIENTED_EDGE ( 'NONE', *, *, #4797, .T. ) ;
#11078 = APPLICATION_PROTOCOL_DEFINITION ( 'draft international standard', 'automotive_design', 1998, #9803 ) ;
#11079 = AXIS2_PLACEMENT_3D ( 'NONE', #14142, #10460, #7659 ) ;
#11080 = CARTESIAN_POINT ( 'NONE',  ( -30.90059672715241845, -91.12516132330414109, 10.00232511491634568 ) ) ;
#11082 = ADVANCED_FACE ( 'NONE', ( #11485 ), #3303, .T. ) ;
#11081 = AXIS2_PLACEMENT_3D ( 'NONE', #13550, #10937, #9518 ) ;
#11083 = DIRECTION ( 'NONE',  ( -0.000000000000000000, -1.000000000000000000, -0.000000000000000000 ) ) ;
#11084 = VERTEX_POINT ( 'NONE', #6013 ) ;
#11085 = CARTESIAN_POINT ( 'NONE',  ( -64.09025127992789805, 84.22855780814606419, 28.00000000000000355 ) ) ;
#11086 = CARTESIAN_POINT ( 'NONE',  ( -98.90286936182231159, -91.08423613455721579, -5.654315315325883162 ) ) ;
#11087 = ADVANCED_FACE ( 'NONE', ( #11642 ), #14365, .F. ) ;
#11088 = CARTESIAN_POINT ( 'NONE',  ( -63.37199650155329778, 75.44273092821040905, -15.00000000000001421 ) ) ;
#11089 = TOROIDAL_SURFACE ( 'NONE', #8393, 4.400000000000000355, 0.4000000000000000222 ) ;
#11090 = ORIENTED_EDGE ( 'NONE', *, *, #12702, .F. ) ;
#11091 = DIRECTION ( 'NONE',  ( -5.204170427930409450E-16, 0.000000000000000000, 1.000000000000000000 ) ) ;
#11092 = CARTESIAN_POINT ( 'NONE',  ( -127.5926225674731995, 117.8748711238780373, -15.00000000000000355 ) ) ;
#11093 = ORIENTED_EDGE ( 'NONE', *, *, #930, .F. ) ;
#11094 = CARTESIAN_POINT ( 'NONE',  ( -171.0109138863553824, 84.22855780814606419, 62.50000000000001421 ) ) ;
#11095 = EDGE_CURVE ( 'NONE', #10929, #535, #3044, .T. ) ;
#11096 = VECTOR ( 'NONE', #4879, 1000.000000000000000 ) ;
#11097 = EDGE_CURVE ( 'NONE', #8646, #15955, #4624, .T. ) ;
#11098 = CARTESIAN_POINT ( 'NONE',  ( -71.24615306438091977, 78.22716831522920700, -167.1454815528550739 ) ) ;
#11099 = EDGE_LOOP ( 'NONE', ( #5074, #6517, #15389, #14480, #3619, #12000 ) ) ;
#11100 = EDGE_CURVE ( 'NONE', #5307, #10700, #7165, .T. ) ;
#11101 = AXIS2_PLACEMENT_3D ( 'NONE', #1267, #18000, #14180 ) ;
#11102 = VECTOR ( 'NONE', #4877, 1000.000000000000000 ) ;
#11103 = CYLINDRICAL_SURFACE ( 'NONE', #4314, 4.599999999999999645 ) ;
#11104 = PLANE ( 'NONE',  #15662 ) ;
#11105 = CARTESIAN_POINT ( 'NONE',  ( -71.24615306438080609, 106.5015021652292404, 15.00000000000006928 ) ) ;
#11106 = ORIENTED_EDGE ( 'NONE', *, *, #137, .T. ) ;
#11107 = EDGE_CURVE ( 'NONE', #12056, #593, #17177, .T. ) ;
#11108 = CARTESIAN_POINT ( 'NONE',  ( -61.98305514952129158, 93.22868410554717400, -167.1454815528550739 ) ) ;
#11109 = CARTESIAN_POINT ( 'NONE',  ( -71.24615306438097662, 60.26648315456372984, 15.00000000000006928 ) ) ;
#11110 = DIRECTION ( 'NONE',  ( 0.9396926207859158664, 0.3420201433256481738, 0.000000000000000000 ) ) ;
#11111 = EDGE_CURVE ( 'NONE', #3038, #18456, #15770, .T. ) ;
#11112 = LINE ( 'NONE', #12800, #12394 ) ;
#11113 = ORIENTED_EDGE ( 'NONE', *, *, #12022, .T. ) ;
#11114 = EDGE_CURVE ( 'NONE', #9668, #889, #16838, .T. ) ;
#11115 = AXIS2_PLACEMENT_3D ( 'NONE', #1779, #7488, #17571 ) ;
#11116 = CARTESIAN_POINT ( 'NONE',  ( -92.59262256747318531, 0.3328663868096687350, -25.00000000000000000 ) ) ;
#11117 = DIRECTION ( 'NONE',  ( 0.9396926207859145341, 0.3420201433256518375, -1.086737899652996918E-16 ) ) ;
#11118 = LINE ( 'NONE', #5304, #12112 ) ;
#11119 = EDGE_CURVE ( 'NONE', #13022, #10671, #320, .T. ) ;
#11120 = CARTESIAN_POINT ( 'NONE',  ( -68.99615306438083451, 95.64293533166268446, -15.00000000000001421 ) ) ;
#11121 = CARTESIAN_POINT ( 'NONE',  ( -68.99615306438097662, 61.70027203813028649, -167.1454815528550739 ) ) ;
#11122 = ORIENTED_EDGE ( 'NONE', *, *, #297, .T. ) ;
#11123 = AXIS2_PLACEMENT_3D ( 'NONE', #17690, #3480, #13590 ) ;
#11124 = FACE_OUTER_BOUND ( 'NONE', #12994, .T. ) ;
#11125 = CARTESIAN_POINT ( 'NONE',  ( -68.99615306438091977, 76.79337943166271430, -167.1454815528550739 ) ) ;
#11126 = EDGE_CURVE ( 'NONE', #4281, #12749, #161, .T. ) ;
#11127 = ADVANCED_FACE ( 'NONE', ( #15855 ), #14627, .T. ) ;
#11128 = CYLINDRICAL_SURFACE ( 'NONE', #2412, 4.599999999999992539 ) ;
#11129 = PLANE ( 'NONE',  #14938 ) ;
#11130 = ORIENTED_EDGE ( 'NONE', *, *, #3097, .F. ) ;
#11131 = VERTEX_POINT ( 'NONE', #8759 ) ;
#11132 = VECTOR ( 'NONE', #16221, 1000.000000000000000 ) ;
#11133 = CARTESIAN_POINT ( 'NONE',  ( 0.2578475836321609260, -6.890627091270527416, -1.065083781909184513 ) ) ;
#11134 = VERTEX_POINT ( 'NONE', #8933 ) ;
#11135 = VECTOR ( 'NONE', #15313, 999.9999999999998863 ) ;
#11136 = DIRECTION ( 'NONE',  ( -0.9396926207859069846, 0.3420201433256723766, -4.890320548438442003E-16 ) ) ;
#11137 = CARTESIAN_POINT ( 'NONE',  ( -74.36154358637296014, 60.48060622302846667, 23.30558296767449278 ) ) ;
#11138 = CARTESIAN_POINT ( 'NONE',  ( -66.00585202009861518, 57.75741913890266943, 25.00000000000001066 ) ) ;
#11139 = ORIENTED_EDGE ( 'NONE', *, *, #7483, .T. ) ;
#11140 = DIRECTION ( 'NONE',  ( -0.000000000000000000, -0.000000000000000000, 1.000000000000000000 ) ) ;
#11141 = CARTESIAN_POINT ( 'NONE',  ( -71.24615306438099083, 35.13374195456380278, 15.00000000000006928 ) ) ;
#11142 = LINE ( 'NONE', #3745, #12011 ) ;
#11143 = ORIENTED_EDGE ( 'NONE', *, *, #6412, .F. ) ;
#11144 = EDGE_CURVE ( 'NONE', #13494, #2247, #7358, .T. ) ;
#11145 = VECTOR ( 'NONE', #9958, 1000.000000000000000 ) ;
#11146 = CARTESIAN_POINT ( 'NONE',  ( -70.85175816390371040, -141.5628872026273086, -57.00000000000000000 ) ) ;
#11147 = EDGE_LOOP ( 'NONE', ( #13555, #10874, #15408, #3468 ) ) ;
#11148 = AXIS2_PLACEMENT_3D ( 'NONE', #4225, #11157, #15738 ) ;
#11149 = DIRECTION ( 'NONE',  ( 0.000000000000000000, 0.000000000000000000, 1.000000000000000000 ) ) ;
#11150 = AXIS2_PLACEMENT_3D ( 'NONE', #13132, #4694, #14452 ) ;
#11151 = DIRECTION ( 'NONE',  ( 0.3420201433256444545, -0.9396926207859171987, 0.000000000000000000 ) ) ;
#11152 = VERTEX_POINT ( 'NONE', #7523 ) ;
#11153 = VERTEX_POINT ( 'NONE', #3144 ) ;
#11154 = VERTEX_POINT ( 'NONE', #14549 ) ;
#11155 = AXIS2_PLACEMENT_3D ( 'NONE', #4463, #10174, #1845 ) ;
#11156 = DIRECTION ( 'NONE',  ( 0.9396926207859158664, 0.3420201433256481738, -1.086737899652998397E-16 ) ) ;
#11157 = DIRECTION ( 'NONE',  ( -1.000000000000000000, -0.000000000000000000, -0.000000000000000000 ) ) ;
#11158 = CARTESIAN_POINT ( 'NONE',  ( -57.08002265617300708, 84.22855780814606419, -15.00000000000001421 ) ) ;
#11159 = DIRECTION ( 'NONE',  ( 0.000000000000000000, 1.000000000000000000, 0.000000000000000000 ) ) ;
#11160 = AXIS2_PLACEMENT_3D ( 'NONE', #15361, #5333, #11053 ) ;
#11161 = DIRECTION ( 'NONE',  ( 0.000000000000000000, 0.000000000000000000, 1.000000000000000000 ) ) ;
#11162 = AXIS2_PLACEMENT_3D ( 'NONE', #5632, #2565, #12570 ) ;
#11163 = CIRCLE ( 'NONE', #7857, 3.999999999999989786 ) ;
#11164 = LINE ( 'NONE', #4055, #7511 ) ;
#11165 = ORIENTED_EDGE ( 'NONE', *, *, #13978, .F. ) ;
#11166 = PLANE ( 'NONE',  #5718 ) ;
#11167 = EDGE_LOOP ( 'NONE', ( #17865, #8185, #8173, #2973 ) ) ;
#11168 = CARTESIAN_POINT ( 'NONE',  ( -68.99615306438091977, 74.26664263813029265, -15.00000000000001421 ) ) ;
#11169 = LINE ( 'NONE', #16860, #11377 ) ;
#11170 = ORIENTED_EDGE ( 'NONE', *, *, #14847, .T. ) ;
#11171 = CARTESIAN_POINT ( 'NONE',  ( -67.59262256747317110, 57.88796029049329661, 26.35917033480641436 ) ) ;
#11172 = EDGE_LOOP ( 'NONE', ( #11547, #2961 ) ) ;
#11173 = PRODUCT_DEFINITION_FORMATION_WITH_SPECIFIED_SOURCE ( 'ANY', '', #6380, .NOT_KNOWN. ) ;
#11174 = CIRCLE ( 'NONE', #8780, 4.599999999999992539 ) ;
#11175 = VECTOR ( 'NONE', #8758, 1000.000000000000000 ) ;
#11176 = EDGE_CURVE ( 'NONE', #11585, #6695, #1724, .T. ) ;
#11177 = VERTEX_POINT ( 'NONE', #13238 ) ;
#11178 = DIRECTION ( 'NONE',  ( 0.000000000000000000, 0.000000000000000000, 1.000000000000000000 ) ) ;
#11179 = CARTESIAN_POINT ( 'NONE',  ( -68.99615306438103346, 32.81108233166271759, -15.00000000000001421 ) ) ;
#11180 = DIRECTION ( 'NONE',  ( -5.204170427930409450E-16, 0.000000000000000000, 1.000000000000000000 ) ) ;
#11181 = VERTEX_POINT ( 'NONE', #418 ) ;
#11182 = APPLICATION_PROTOCOL_DEFINITION ( 'draft international standard', 'automotive_design', 1998, #3944 ) ;
#11183 = VERTEX_POINT ( 'NONE', #12247 ) ;
#11184 = DIRECTION ( 'NONE',  ( 0.000000000000000000, 0.000000000000000000, 1.000000000000000000 ) ) ;
#11185 = CARTESIAN_POINT ( 'NONE',  ( 95.45835937779683888, -32.62665103886254059, -7.000000000000010658 ) ) ;
#11186 = ORIENTED_EDGE ( 'NONE', *, *, #10626, .F. ) ;
#11187 = CARTESIAN_POINT ( 'NONE',  ( -68.99615306438111872, 13.96152643166267993, 15.00000000000006928 ) ) ;
#11188 = CARTESIAN_POINT ( 'NONE',  ( -71.24615306438114715, 15.39531531522927921, -167.1454815528550739 ) ) ;
#11189 = ORIENTED_EDGE ( 'NONE', *, *, #931, .F. ) ;
#11190 = DIRECTION ( 'NONE',  ( -1.000000000000000000, 0.000000000000000000, 0.000000000000000000 ) ) ;
#11191 = VECTOR ( 'NONE', #3070, 1000.000000000000000 ) ;
#11192 = ORIENTED_EDGE ( 'NONE', *, *, #4129, .T. ) ;
#11193 = DIRECTION ( 'NONE',  ( 1.000000000000000000, 0.000000000000000000, 0.000000000000000000 ) ) ;
#11194 = CARTESIAN_POINT ( 'NONE',  ( -66.51364668169603078, 112.0410723289543995, -28.00000000000000355 ) ) ;
#11195 = ORIENTED_EDGE ( 'NONE', *, *, #12142, .T. ) ;
#11196 = B_SPLINE_CURVE_WITH_KNOTS ( 'NONE', 3,
 ( #15537, #8338, #15645, #2729 ),
 .UNSPECIFIED., .F., .F.,
 ( 4, 4 ),
 ( 0.01093108579351914633, 0.01364771765276243456 ),
 .UNSPECIFIED. ) ;
#11197 = LINE ( 'NONE', #8383, #13605 ) ;
#11198 = AXIS2_PLACEMENT_3D ( 'NONE', #12196, #6572, #17803 ) ;
#11199 = CARTESIAN_POINT ( 'NONE',  ( -66.17203968311494577, 56.30249863064624094, -26.82861026404109239 ) ) ;
#11200 = ORIENTED_EDGE ( 'NONE', *, *, #12738, .F. ) ;
#11201 = VECTOR ( 'NONE', #2309, 1000.000000000000000 ) ;
#11202 = EDGE_CURVE ( 'NONE', #2538, #7201, #3741, .T. ) ;
#11203 = CIRCLE ( 'NONE', #6389, 5.000000000000000888 ) ;
#11204 = AXIS2_PLACEMENT_3D ( 'NONE', #13959, #1141, #18258 ) ;
#11205 = PRODUCT_DEFINITION_SHAPE ( 'NONE', 'NONE',  #3491 ) ;
#11206 = ORIENTED_EDGE ( 'NONE', *, *, #6061, .F. ) ;
#11207 = CYLINDRICAL_SURFACE ( 'NONE', #18036, 22.04359719766050318 ) ;
#11208 = EDGE_LOOP ( 'NONE', ( #1362, #14994, #14974, #2441, #5966, #15780, #18145, #15111, #2109, #5569, #7422, #12877, #14571, #508, #16136, #10961, #12450, #16911, #9833, #8542, #16006, #13016, #5176, #4690, #1522, #11606, #8484, #3581, #7140, #12980, #10070, #10103, #15901, #9645, #5788, #4131, #5104, #17335, #17125, #3516, #12930, #11186, #54, #6835, #17652, #13105, #5092, #12370, #14910, #14411, #1671, #15447, #12572, #2625, #14003, #8247, #15683, #2967, #7246, #9131, #12508, #5311, #6451, #4241, #5239, #13773, #6366, #13173, #15568, #10051, #17185, #8978, #6033, #16679, #18210, #10195, #12388, #15016, #3347, #2854, #10836, #6436, #13244, #10789, #2593, #16887, #9913, #12293, #2656, #12773, #3895, #9743, #6233, #6595, #17897, #10892, #16767, #4834, #6945, #13785, #13532, #10788, #12239, #15484, #17072, #2564, #10757, #16316, #7690, #15490, #9409, #4862, #1467, #18400, #8620, #1718, #7846, #7053, #12675, #14109, #7410, #2230, #7021, #7565, #2413, #7701, #14882, #382, #4752, #14893, #12768, #3161, #10750, #9943, #8221, #12138, #16639, #4365, #14437, #2399, #6256, #339, #8749, #8371, #5601, #8951, #6164, #783, #14277, #10799, #14087, #7862, #17328, #12756, #4883, #9900, #12715, #8558, #7018, #16966, #10047, #6113, #16257, #14065, #13084, #7498, #3986, #15940, #9941, #16818, #12647, #10773, #6858, #3813, #1776, #7514, #15511, #4903, #18475, #4415, #11922, #12735, #18411, #2253, #7299, #5729, #4204, #1547, #10044, #521, #16407, #7656, #11200, #2753, #14377, #4571, #4484 ) ) ;
#11209 = DIRECTION ( 'NONE',  ( -1.156482317317869999E-16, 0.000000000000000000, -1.000000000000000000 ) ) ;
#11210 = LINE ( 'NONE', #5298, #6540 ) ;
#11211 = DIRECTION ( 'NONE',  ( 1.156482317317869999E-16, 0.000000000000000000, 1.000000000000000000 ) ) ;
#11212 = CARTESIAN_POINT ( 'NONE',  ( -59.35080917176598092, 94.79374675277695417, -15.00000000000001421 ) ) ;
#11213 = VERTEX_POINT ( 'NONE', #6444 ) ;
#11214 = AXIS2_PLACEMENT_3D ( 'NONE', #6084, #5990, #1891 ) ;
#11215 = EDGE_CURVE ( 'NONE', #4466, #2953, #1124, .T. ) ;
#11216 = FACE_OUTER_BOUND ( 'NONE', #7458, .T. ) ;
#11217 = DIRECTION ( 'NONE',  ( 0.3420201433256637724, -0.9396926207859102043, 0.000000000000000000 ) ) ;
#11218 = DIRECTION ( 'NONE',  ( -1.000000000000000000, -4.218847493575593591E-14, 1.387778780781445182E-16 ) ) ;
#11219 = CARTESIAN_POINT ( 'NONE',  ( -10.92059662857647240, 26.05810099730991070, -40.87008517519171136 ) ) ;
#11220 = DIRECTION ( 'NONE',  ( 0.000000000000000000, 0.000000000000000000, 1.000000000000000000 ) ) ;
#11221 = ORIENTED_EDGE ( 'NONE', *, *, #4048, .F. ) ;
#11222 = CIRCLE ( 'NONE', #15090, 17.12963335357822814 ) ;
#11223 = AXIS2_PLACEMENT_3D ( 'NONE', #14592, #11799, #3357 ) ;
#11224 = VECTOR ( 'NONE', #4028, 1000.000000000000000 ) ;
#11225 = CARTESIAN_POINT ( 'NONE',  ( -68.99615306438087714, 67.98345733813025049, -15.00000000000001421 ) ) ;
#11226 = CARTESIAN_POINT ( 'NONE',  ( -77.38579898953862823, 74.98691627113693414, 97.49999999999998579 ) ) ;
#11227 = LINE ( 'NONE', #6811, #898 ) ;
#11228 = EDGE_CURVE ( 'NONE', #10691, #703, #9446, .T. ) ;
#11229 = CARTESIAN_POINT ( 'NONE',  ( 0.000000000000000000, 2.678141147339130316E-16, -4.000000000000024869 ) ) ;
#11230 = VERTEX_POINT ( 'NONE', #9733 ) ;
#11231 = EDGE_CURVE ( 'NONE', #10424, #9440, #15434, .T. ) ;
#11232 = EDGE_LOOP ( 'NONE', ( #3856, #2956, #4985, #17799, #10239, #13288 ) ) ;
#11233 = EDGE_CURVE ( 'NONE', #17254, #3060, #4037, .T. ) ;
#11234 = FACE_BOUND ( 'NONE', #17686, .T. ) ;
#11235 = AXIS2_PLACEMENT_3D ( 'NONE', #11094, #2674, #6692 ) ;
#11236 = MECHANICAL_DESIGN_GEOMETRIC_PRESENTATION_REPRESENTATION (  '', ( #16892 ), #2251 ) ;
#11237 = CIRCLE ( 'NONE', #7057, 3.999999999999996447 ) ;
#11238 = CARTESIAN_POINT ( 'NONE',  ( -67.15841416737785607, 56.64230282782159520, 23.31749251357070918 ) ) ;
#11239 = CARTESIAN_POINT ( 'NONE',  ( -123.4618227840623632, -111.0842361345572158, -18.23991632971910803 ) ) ;
#11240 = CARTESIAN_POINT ( 'NONE',  ( -60.19468178563322169, -91.08423613455723000, -39.14310232490480956 ) ) ;
#11241 = ORIENTED_EDGE ( 'NONE', *, *, #10104, .F. ) ;
#11242 = EDGE_CURVE ( 'NONE', #1357, #1661, #4869, .T. ) ;
#11243 = EDGE_CURVE ( 'NONE', #1357, #12287, #17720, .T. ) ;
#11244 = CARTESIAN_POINT ( 'NONE',  ( -66.47936379154189979, 109.1731751823756014, -28.00000000000000000 ) ) ;
#11245 = EDGE_CURVE ( 'NONE', #513, #14058, #836, .T. ) ;
#11246 = CARTESIAN_POINT ( 'NONE',  ( -76.37409655828265898, -91.08423613455721579, -8.001217251689905290E-13 ) ) ;
#11247 = CARTESIAN_POINT ( 'NONE',  ( 9.543663295069050534, 56.41207303426870112, 3.000000000000000000 ) ) ;
#11248 = VERTEX_POINT ( 'NONE', #13843 ) ;
#11249 = EDGE_CURVE ( 'NONE', #17198, #8524, #13940, .T. ) ;
#11250 = CARTESIAN_POINT ( 'NONE',  ( -71.24615306438099083, 53.98329785456374452, -15.00000000000001421 ) ) ;
#11251 = ORIENTED_EDGE ( 'NONE', *, *, #2375, .T. ) ;
#11252 = EDGE_CURVE ( 'NONE', #5754, #5470, #6822, .T. ) ;
#11253 = CARTESIAN_POINT ( 'NONE',  ( -97.59262256747321373, 114.3311569208253786, -25.00000000000000000 ) ) ;
#11254 = DIRECTION ( 'NONE',  ( 0.000000000000000000, 1.000000000000000000, 0.000000000000000000 ) ) ;
#11255 = ORIENTED_EDGE ( 'NONE', *, *, #6641, .F. ) ;
#11256 = ORIENTED_EDGE ( 'NONE', *, *, #13063, .F. ) ;
#11257 = EDGE_CURVE ( 'NONE', #8404, #13480, #16441, .T. ) ;
#11258 = EDGE_CURVE ( 'NONE', #7872, #3710, #13658, .T. ) ;
#11259 = ORIENTED_EDGE ( 'NONE', *, *, #13138, .T. ) ;
#11260 = DIRECTION ( 'NONE',  ( -0.9396926207859158664, 0.3420201433256481738, 0.000000000000000000 ) ) ;
#11261 = PLANE ( 'NONE',  #15635 ) ;
#11262 = CARTESIAN_POINT ( 'NONE',  ( -107.5926225674731711, 57.88796029049330372, 26.35917033480641436 ) ) ;
#11263 = DIRECTION ( 'NONE',  ( -0.9396926207859093161, 0.3420201433256663814, -4.890320548438453836E-16 ) ) ;
#11264 = PLANE ( 'NONE',  #6936 ) ;
#11265 = EDGE_CURVE ( 'NONE', #15284, #16629, #14936, .T. ) ;
#11266 = ORIENTED_EDGE ( 'NONE', *, *, #17045, .F. ) ;
#11267 = CARTESIAN_POINT ( 'NONE',  ( -67.02098183716937285, 79.99098546104525553, 15.00000000000006928 ) ) ;
#11268 = ORIENTED_EDGE ( 'NONE', *, *, #1689, .F. ) ;
#11269 = DIRECTION ( 'NONE',  ( -1.000000000000000000, -0.000000000000000000, -0.000000000000000000 ) ) ;
#11270 = B_SPLINE_CURVE_WITH_KNOTS ( 'NONE', 3,
 ( #9228, #726, #6418, #2212, #12141, #16416, #7925, #12220, #17916, #16517, #3715, #9425, #15120, #13716, #18314, #9893, #63, #9992, #6800, #16902, #15700, #11395, #18217, #9796, #2497, #15601 ),
 .UNSPECIFIED., .F., .F.,
 ( 4, 2, 2, 2, 2, 2, 2, 2, 2, 2, 2, 2, 4 ),
 ( 6.992893892674702526E-18, 0.01247275093652063134, 0.01870912640478094788, 0.02182731413891110528, 0.02494550187304126268, 0.03741825280956187494, 0.04365462827782218974, 0.04677281601195235755, 0.04989100374608251842, 0.06236375468260317578, 0.07483650561912381927, 0.08730925655564447663, 0.09978200749216512011 ),
 .UNSPECIFIED. ) ;
#11271 = DIRECTION ( 'NONE',  ( -5.204170427930409450E-16, 0.000000000000000000, 1.000000000000000000 ) ) ;
#11272 = ORIENTED_EDGE ( 'NONE', *, *, #12503, .T. ) ;
#11273 = DIRECTION ( 'NONE',  ( 0.3420201433256802037, -0.9396926207859043201, 0.000000000000000000 ) ) ;
#11274 = ORIENTED_EDGE ( 'NONE', *, *, #3420, .F. ) ;
#11275 = VERTEX_POINT ( 'NONE', #16632 ) ;
#11276 = DIRECTION ( 'NONE',  ( -1.000000000000000000, 0.000000000000000000, 0.000000000000000000 ) ) ;
#11277 = DIRECTION ( 'NONE',  ( 0.000000000000000000, 0.000000000000000000, -1.000000000000000000 ) ) ;
#11278 = VERTEX_POINT ( 'NONE', #2422 ) ;
#11279 = CONTEXT_DEPENDENT_SHAPE_REPRESENTATION ( #1440, #1039 ) ;
#11280 = EDGE_LOOP ( 'NONE', ( #5953, #200, #5413, #13530 ) ) ;
#11281 = CARTESIAN_POINT ( 'NONE',  ( -71.24615306438083451, 97.96559495456375544, -167.1454815528550739 ) ) ;
#11282 = CARTESIAN_POINT ( 'NONE',  ( -71.24615306438111872, 22.56737135456379661, 15.00000000000006928 ) ) ;
#11283 = ORIENTED_EDGE ( 'NONE', *, *, #17501, .T. ) ;
#11284 = CARTESIAN_POINT ( 'NONE',  ( -64.09025127992791226, 109.3109350805793270, 28.00000000000000355 ) ) ;
#11285 = DIRECTION ( 'NONE',  ( 0.000000000000000000, 1.000000000000000000, 0.000000000000000000 ) ) ;
#11286 = DIRECTION ( 'NONE',  ( 0.000000000000000000, 0.000000000000000000, -1.000000000000000000 ) ) ;
#11287 = VERTEX_POINT ( 'NONE', #12453 ) ;
#11288 = DIRECTION ( 'NONE',  ( -0.000000000000000000, -0.000000000000000000, 1.000000000000000000 ) ) ;
#11289 = LINE ( 'NONE', #13801, #1298 ) ;
#11291 = ORIENTED_EDGE ( 'NONE', *, *, #5471, .T. ) ;
#11290 = ADVANCED_FACE ( 'NONE', ( #18148 ), #8231, .T. ) ;
#11292 = FACE_OUTER_BOUND ( 'NONE', #16428, .T. ) ;
#11293 = VERTEX_POINT ( 'NONE', #11322 ) ;
#11294 = EDGE_CURVE ( 'NONE', #18326, #9028, #7013, .T. ) ;
#11295 = CARTESIAN_POINT ( 'NONE',  ( -67.13578943540532862, 56.63396920285576641, -23.36002886201060846 ) ) ;
#11296 = ORIENTED_EDGE ( 'NONE', *, *, #8452, .T. ) ;
#11297 = CARTESIAN_POINT ( 'NONE',  ( -71.24615306438083451, 97.07672421522921979, -167.1454815528550739 ) ) ;
#11298 = DIRECTION ( 'NONE',  ( -0.9396926207859093161, 0.3420201433256661039, -4.890320548438453836E-16 ) ) ;
#11299 = ORIENTED_EDGE ( 'NONE', *, *, #15515, .T. ) ;
#11300 = LINE ( 'NONE', #10245, #9859 ) ;
#11301 = LINE ( 'NONE', #15302, #7727 ) ;
#11302 = PLANE ( 'NONE',  #12969 ) ;
#11303 = DIRECTION ( 'NONE',  ( -0.9396926207859145341, 0.3420201433256519485, 0.000000000000000000 ) ) ;
#11304 = ORIENTED_EDGE ( 'NONE', *, *, #2752, .T. ) ;
#11305 = DIRECTION ( 'NONE',  ( -1.000000000000000000, 0.000000000000000000, 0.000000000000000000 ) ) ;
#11306 = PLANE ( 'NONE',  #3399 ) ;
#11307 = CARTESIAN_POINT ( 'NONE',  ( -34.76410658286479816, 45.09554562204261430, -30.51224260568122304 ) ) ;
#11308 = CARTESIAN_POINT ( 'NONE',  ( -68.99615306438077766, 118.2489397381302751, -167.1454815528550739 ) ) ;
#11309 = ORIENTED_EDGE ( 'NONE', *, *, #12235, .T. ) ;
#11310 = PLANE ( 'NONE',  #9414 ) ;
#11311 = DIRECTION ( 'NONE',  ( 0.000000000000000000, 0.000000000000000000, -1.000000000000000000 ) ) ;
#11312 = LINE ( 'NONE', #17002, #29 ) ;
#11313 = LINE ( 'NONE', #6909, #12267 ) ;
#11314 = EDGE_LOOP ( 'NONE', ( #7864, #17434 ) ) ;
#11315 = ORIENTED_EDGE ( 'NONE', *, *, #6375, .T. ) ;
#11316 = EDGE_CURVE ( 'NONE', #6650, #4400, #12914, .T. ) ;
#11317 = CARTESIAN_POINT ( 'NONE',  ( -47.19781944808393348, 88.60139997190906058, -15.00000000000001421 ) ) ;
#11318 = ORIENTED_EDGE ( 'NONE', *, *, #13073, .T. ) ;
#11319 = CARTESIAN_POINT ( 'NONE',  ( -107.5926225674731853, 110.5691553257988460, 22.33417033480641223 ) ) ;
#11320 = LINE ( 'NONE', #4202, #3082 ) ;
#11321 = AXIS2_PLACEMENT_3D ( 'NONE', #10692, #7614, #11911 ) ;
#11322 = CARTESIAN_POINT ( 'NONE',  ( -71.24615306438100504, 49.95283446522918780, -15.00000000000001421 ) ) ;
#11323 = ORIENTED_EDGE ( 'NONE', *, *, #15890, .T. ) ;
#11324 = FACE_OUTER_BOUND ( 'NONE', #15660, .T. ) ;
#11325 = CARTESIAN_POINT ( 'NONE',  ( -92.59262256747321373, 117.8748711238780373, 15.00000000000006040 ) ) ;
#11326 = PLANE ( 'NONE',  #15080 ) ;
#11327 = DIRECTION ( 'NONE',  ( 0.000000000000000000, 1.000000000000000000, 2.775557561562874095E-16 ) ) ;
#11328 = ORIENTED_EDGE ( 'NONE', *, *, #7562, .T. ) ;
#11329 = EDGE_CURVE ( 'NONE', #11975, #2362, #10570, .T. ) ;
#11330 = CARTESIAN_POINT ( 'NONE',  ( -71.24615306438070661, 138.8062994045637311, 15.00000000000006928 ) ) ;
#11331 = VERTEX_POINT ( 'NONE', #11592 ) ;
#11332 = CARTESIAN_POINT ( 'NONE',  ( -51.81614838398844824, 95.01461175692088545, -167.1454815528550739 ) ) ;
#11333 = LINE ( 'NONE', #11527, #10709 ) ;
#11334 = ORIENTED_EDGE ( 'NONE', *, *, #2706, .F. ) ;
#11335 = AXIS2_PLACEMENT_3D ( 'NONE', #8041, #1229, #12264 ) ;
#11336 = EDGE_LOOP ( 'NONE', ( #15544, #11528, #13808, #4676 ) ) ;
#11337 = EDGE_CURVE ( 'NONE', #13685, #6726, #902, .T. ) ;
#11338 = ADVANCED_FACE ( 'NONE', ( #8523, #17281 ), #4465, .T. ) ;
#11339 = VERTEX_POINT ( 'NONE', #88 ) ;
#11340 = CARTESIAN_POINT ( 'NONE',  ( -71.24615306438091977, 78.22716831522920700, -15.00000000000001421 ) ) ;
#11341 = FACE_OUTER_BOUND ( 'NONE', #4235, .T. ) ;
#11342 = CARTESIAN_POINT ( 'NONE',  ( -68.99615306438070661, 136.4836397816626743, -15.00000000000001421 ) ) ;
#11343 = EDGE_CURVE ( 'NONE', #4543, #1922, #5503, .T. ) ;
#11344 = DIRECTION ( 'NONE',  ( -1.224646799147353207E-16, 1.000000000000000000, 0.000000000000000000 ) ) ;
#11345 = CARTESIAN_POINT ( 'NONE',  ( -67.88623620617454435, 84.15481808402788033, -15.00000000000001421 ) ) ;
#11346 = EDGE_LOOP ( 'NONE', ( #5989, #11634, #14262, #13714 ) ) ;
#11348 = EDGE_CURVE ( 'NONE', #4697, #10024, #4388, .T. ) ;
#11347 = VECTOR ( 'NONE', #5101, 1000.000000000000000 ) ;
#11349 = CARTESIAN_POINT ( 'NONE',  ( -68.99615306438080609, 108.8241617881302545, 15.00000000000006928 ) ) ;
#11350 = ORIENTED_EDGE ( 'NONE', *, *, #8517, .F. ) ;
#11351 = CARTESIAN_POINT ( 'NONE',  ( -68.99615306438083451, 98.78452798166264870, 15.00000000000006928 ) ) ;
#11352 = AXIS2_PLACEMENT_3D ( 'NONE', #10163, #176, #6204 ) ;
#11353 = EDGE_CURVE ( 'NONE', #8311, #13617, #6917, .T. ) ;
#11354 = EDGE_CURVE ( 'NONE', #7696, #16406, #6212, .T. ) ;
#11355 = DIRECTION ( 'NONE',  ( -0.000000000000000000, -0.000000000000000000, -1.000000000000000000 ) ) ;
#11356 = VERTEX_POINT ( 'NONE', #1320 ) ;
#11357 = CARTESIAN_POINT ( 'NONE',  ( -112.3460510726626040, -91.53393135689863414, -8.561720054222236698 ) ) ;
#11358 = ORIENTED_EDGE ( 'NONE', *, *, #13741, .T. ) ;
#11359 = ADVANCED_FACE ( 'NONE', ( #5872 ), #7024, .T. ) ;
#11360 = AXIS2_PLACEMENT_3D ( 'NONE', #11633, #2947, #8651 ) ;
#11361 = ORIENTED_EDGE ( 'NONE', *, *, #9320, .T. ) ;
#11362 = AXIS2_PLACEMENT_3D ( 'NONE', #14883, #18166, #10871 ) ;
#11363 = DIRECTION ( 'NONE',  ( 1.156482317317869999E-16, 0.000000000000000000, 1.000000000000000000 ) ) ;
#11364 =( REPRESENTATION_RELATIONSHIP ('NONE','NONE', #359, #13055 ) REPRESENTATION_RELATIONSHIP_WITH_TRANSFORMATION ( #15569 )SHAPE_REPRESENTATION_RELATIONSHIP( ) );
#11365 = DIRECTION ( 'NONE',  ( 0.000000000000000000, 0.000000000000000000, -1.000000000000000000 ) ) ;
#11366 = PLANE ( 'NONE',  #379 ) ;
#11367 = ORIENTED_EDGE ( 'NONE', *, *, #17960, .T. ) ;
#11368 = CONTEXT_DEPENDENT_SHAPE_REPRESENTATION ( #2998, #4032 ) ;
#11369 = VERTEX_POINT ( 'NONE', #4299 ) ;
#11370 = CARTESIAN_POINT ( 'NONE',  ( -12.34732335292710559, 42.05992578482485555, -32.40189210255460495 ) ) ;
#11371 = CARTESIAN_POINT ( 'NONE',  ( -71.24615306438109030, 31.10327856522923540, 15.00000000000006928 ) ) ;
#11372 = EDGE_LOOP ( 'NONE', ( #14308, #3486 ) ) ;
#11373 = DIRECTION ( 'NONE',  ( 0.9396926207859084279, 0.3420201433256686574, 4.890320548438448905E-16 ) ) ;
#11374 = DIRECTION ( 'NONE',  ( -5.204170427930409450E-16, 0.000000000000000000, 1.000000000000000000 ) ) ;
#11375 = DIRECTION ( 'NONE',  ( 0.000000000000000000, 0.000000000000000000, 1.000000000000000000 ) ) ;
#11376 = VERTEX_POINT ( 'NONE', #10013 ) ;
#11377 = VECTOR ( 'NONE', #6563, 1000.000000000000000 ) ;
#11378 = ADVANCED_FACE ( 'NONE', ( #15724 ), #8606, .T. ) ;
#11379 = PLANE ( 'NONE',  #14041 ) ;
#11380 = ORIENTED_EDGE ( 'NONE', *, *, #14526, .T. ) ;
#11381 = VECTOR ( 'NONE', #16633, 1000.000000000000000 ) ;
#11382 = ORIENTED_EDGE ( 'NONE', *, *, #16823, .F. ) ;
#11383 = VECTOR ( 'NONE', #7568, 1000.000000000000000 ) ;
#11384 = DIRECTION ( 'NONE',  ( 0.000000000000000000, 1.000000000000000000, 0.000000000000000000 ) ) ;
#11385 = ORIENTED_EDGE ( 'NONE', *, *, #12147, .F. ) ;
#11386 = VECTOR ( 'NONE', #12734, 1000.000000000000000 ) ;
#11387 = EDGE_LOOP ( 'NONE', ( #1959, #4546, #7389, #3449 ) ) ;
#11388 = AXIS2_PLACEMENT_3D ( 'NONE', #7118, #2719, #12826 ) ;
#11389 = DIRECTION ( 'NONE',  ( 0.9396926207859158664, 0.3420201433256481738, 0.000000000000000000 ) ) ;
#11390 = VERTEX_POINT ( 'NONE', #350 ) ;
#11391 = VECTOR ( 'NONE', #12991, 1000.000000000000000 ) ;
#11392 = DIRECTION ( 'NONE',  ( 1.000000000000000000, 0.000000000000000000, 0.000000000000000000 ) ) ;
#11393 = CARTESIAN_POINT ( 'NONE',  ( 5.299999999999998934, -3.752776749732712691, -6.500000000000033751 ) ) ;
#11394 = AXIS2_PLACEMENT_3D ( 'NONE', #4092, #11209, #6704 ) ;
#11395 = CARTESIAN_POINT ( 'NONE',  ( -31.19111409321185846, 43.29857725109086175, 31.64380382776071343 ) ) ;
#11396 = DIRECTION ( 'NONE',  ( 1.000000000000000000, -0.000000000000000000, -0.000000000000000000 ) ) ;
#11397 = ORIENTED_EDGE ( 'NONE', *, *, #16938, .F. ) ;
#11398 = CARTESIAN_POINT ( 'NONE',  ( -71.24615306438089135, 84.51035361522924916, -15.00000000000001421 ) ) ;
#11399 = FACE_OUTER_BOUND ( 'NONE', #4960, .T. ) ;
#11400 = FACE_OUTER_BOUND ( 'NONE', #14278, .T. ) ;
#11401 = ORIENTED_EDGE ( 'NONE', *, *, #6991, .T. ) ;
#11402 = VECTOR ( 'NONE', #16675, 1000.000000000000000 ) ;
#11403 = LINE ( 'NONE', #12731, #1644 ) ;
#11404 = DIRECTION ( 'NONE',  ( 1.000000000000000000, 0.000000000000000000, 0.000000000000000000 ) ) ;
#11405 = DIRECTION ( 'NONE',  ( 1.000000000000000000, 2.062304371594500494E-16, -0.000000000000000000 ) ) ;
#11406 = VECTOR ( 'NONE', #15104, 1000.000000000000000 ) ;
#11407 = AXIS2_PLACEMENT_3D ( 'NONE', #8664, #6111, #11838 ) ;
#11408 = DIRECTION ( 'NONE',  ( 1.000000000000000000, 0.000000000000000000, 6.950654929607132427E-15 ) ) ;
#11409 = EDGE_LOOP ( 'NONE', ( #2588, #10737, #16039, #9024 ) ) ;
#11410 = VERTEX_POINT ( 'NONE', #527 ) ;
#11412 = ADVANCED_FACE ( 'NONE', ( #6039 ), #8963, .T. ) ;
#11411 = DIRECTION ( 'NONE',  ( -0.7071067811865474617, 0.000000000000000000, 0.7071067811865474617 ) ) ;
#11413 = AXIS2_PLACEMENT_3D ( 'NONE', #7224, #3014, #8724 ) ;
#11414 = EDGE_LOOP ( 'NONE', ( #9155, #16715, #16796, #3359, #11933 ) ) ;
#11415 = CARTESIAN_POINT ( 'NONE',  ( -67.13594510831309492, 111.8230895504084117, -23.35973016812594949 ) ) ;
#11416 = DIRECTION ( 'NONE',  ( 0.000000000000000000, 0.000000000000000000, -1.000000000000000000 ) ) ;
#11417 = ORIENTED_EDGE ( 'NONE', *, *, #17269, .F. ) ;
#11418 = CARTESIAN_POINT ( 'NONE',  ( -66.18295968148926534, 110.2709693283236874, -28.00000000000000000 ) ) ;
#11419 = AXIS2_PLACEMENT_3D ( 'NONE', #9011, #3667, #11903 ) ;
#11420 = DIRECTION ( 'NONE',  ( 0.000000000000000000, 0.000000000000000000, -1.000000000000000000 ) ) ;
#11421 = CARTESIAN_POINT ( 'NONE',  ( -71.24615306438103346, 41.41692725456378099, -15.00000000000001421 ) ) ;
#11422 = EDGE_LOOP ( 'NONE', ( #9563, #18375, #6925, #1685 ) ) ;
#11423 = LINE ( 'NONE', #7968, #5724 ) ;
#11424 = PLANE ( 'NONE',  #11388 ) ;
#11425 = VERTEX_POINT ( 'NONE', #1752 ) ;
#11426 = AXIS2_PLACEMENT_3D ( 'NONE', #10521, #2103, #10804 ) ;
#11427 = CARTESIAN_POINT ( 'NONE',  ( 4.699999999999995737, 6.499999999999901412, 2.428612866367529932E-14 ) ) ;
#11428 = DIRECTION ( 'NONE',  ( -0.000000000000000000, -0.000000000000000000, 1.000000000000000000 ) ) ;
#11429 = VERTEX_POINT ( 'NONE', #5952 ) ;
#11430 = ORIENTED_EDGE ( 'NONE', *, *, #16169, .T. ) ;
#11431 = AXIS2_PLACEMENT_3D ( 'NONE', #9899, #8505, #5673 ) ;
#11432 = VECTOR ( 'NONE', #189, 1000.000000000000000 ) ;
#11433 = ORIENTED_EDGE ( 'NONE', *, *, #17733, .F. ) ;
#11434 = EDGE_CURVE ( 'NONE', #13472, #14911, #2024, .T. ) ;
#11435 = CARTESIAN_POINT ( 'NONE',  ( -66.88945454405379110, 81.25920652595873150, -15.00000000000001421 ) ) ;
#11436 = CARTESIAN_POINT ( 'NONE',  ( -71.24615306438117557, 5.970537365229261262, -15.00000000000001421 ) ) ;
#11437 = CARTESIAN_POINT ( 'NONE',  ( 95.45835937779679625, 56.41207303426869402, -7.000000000000010658 ) ) ;
#11438 = CIRCLE ( 'NONE', #3651, 12.49999999999999112 ) ;
#11439 = DIRECTION ( 'NONE',  ( 0.000000000000000000, 0.000000000000000000, 1.000000000000000000 ) ) ;
#11440 = CARTESIAN_POINT ( 'NONE',  ( -123.4618227840623632, -111.0842361345572158, -57.00000000000000000 ) ) ;
#11441 = ORIENTED_EDGE ( 'NONE', *, *, #12137, .T. ) ;
#11442 = CARTESIAN_POINT ( 'NONE',  ( 124.5381772159375942, -111.0842361345572158, 7.000000000000010658 ) ) ;
#11443 = ORIENTED_EDGE ( 'NONE', *, *, #10420, .F. ) ;
#11444 = EDGE_CURVE ( 'NONE', #848, #4970, #4825, .T. ) ;
#11445 = CARTESIAN_POINT ( 'NONE',  ( -71.24615306438066398, 129.3815214545637389, 15.00000000000006928 ) ) ;
#11446 = CIRCLE ( 'NONE', #974, 4.600000000000006750 ) ;
#11447 = VECTOR ( 'NONE', #13779, 1000.000000000000000 ) ;
#11448 = DIRECTION ( 'NONE',  ( 0.000000000000000000, 0.000000000000000000, 1.000000000000000000 ) ) ;
#11450 = EDGE_CURVE ( 'NONE', #6999, #3974, #10546, .T. ) ;
#11449 = EDGE_LOOP ( 'NONE', ( #12854, #12979, #13081, #9708 ) ) ;
#11451 = DIRECTION ( 'NONE',  ( -0.9396926207859157554, 0.3420201433256481738, -4.890320548438487362E-16 ) ) ;
#11452 = VERTEX_POINT ( 'NONE', #4650 ) ;
#11453 = VECTOR ( 'NONE', #15363, 1000.000000000000000 ) ;
#11454 = EDGE_CURVE ( 'NONE', #11183, #14076, #16054, .T. ) ;
#11455 = ADVANCED_FACE ( 'NONE', ( #17544 ), #8785, .T. ) ;
#11456 = ORIENTED_EDGE ( 'NONE', *, *, #150, .F. ) ;
#11457 = EDGE_CURVE ( 'NONE', #16207, #18159, #1020, .T. ) ;
#11458 = CIRCLE ( 'NONE', #16203, 3.999999999999989786 ) ;
#11459 = CIRCLE ( 'NONE', #16205, 4.599999999999999645 ) ;
#11460 = CARTESIAN_POINT ( 'NONE',  ( -68.76426085488260753, 88.67024416760638417, -15.00000000000001421 ) ) ;
#11461 = DIRECTION ( 'NONE',  ( -2.062304371594500494E-16, 1.000000000000000000, -0.000000000000000000 ) ) ;
#11462 = CARTESIAN_POINT ( 'NONE',  ( -68.99615306438083451, 98.78452798166264870, -167.1454815528550739 ) ) ;
#11463 = ORIENTED_EDGE ( 'NONE', *, *, #8374, .T. ) ;
#11464 = CARTESIAN_POINT ( 'NONE',  ( -26.55110732739451507, -93.39009773859100960, 6.425137615056152995 ) ) ;
#11465 = DIRECTION ( 'NONE',  ( -1.000000000000000000, 0.000000000000000000, 0.000000000000000000 ) ) ;
#11466 = VERTEX_POINT ( 'NONE', #11768 ) ;
#11467 = EDGE_CURVE ( 'NONE', #6109, #16861, #5790, .T. ) ;
#11468 = TOROIDAL_SURFACE ( 'NONE', #4867, 10.04359719766049963, 1.000000000000000000 ) ;
#11469 = DIRECTION ( 'NONE',  ( 1.156482317317869999E-16, 0.000000000000000000, 1.000000000000000000 ) ) ;
#11470 = DIRECTION ( 'NONE',  ( 1.000000000000000000, 0.000000000000000000, 5.077734830647302671E-16 ) ) ;
#11471 = ADVANCED_FACE ( 'NONE', ( #9146 ), #1670, .T. ) ;
#11472 = DIRECTION ( 'NONE',  ( 0.000000000000000000, 1.000000000000000000, -0.000000000000000000 ) ) ;
#11473 = EDGE_CURVE ( 'NONE', #845, #12461, #2511, .T. ) ;
#11474 = VERTEX_POINT ( 'NONE', #17363 ) ;
#11475 = DIRECTION ( 'NONE',  ( 0.000000000000000000, 0.000000000000000000, 1.000000000000000000 ) ) ;
#11476 = ORIENTED_EDGE ( 'NONE', *, *, #716, .F. ) ;
#11477 = EDGE_CURVE ( 'NONE', #288, #13807, #10271, .T. ) ;
#11478 =( GEOMETRIC_REPRESENTATION_CONTEXT ( 3 ) GLOBAL_UNCERTAINTY_ASSIGNED_CONTEXT ( ( #15252 ) ) GLOBAL_UNIT_ASSIGNED_CONTEXT ( ( #14833, #5005, #13539 ) ) REPRESENTATION_CONTEXT ( 'NONE', 'WORKASPACE' ) );
#11479 = ORIENTED_EDGE ( 'NONE', *, *, #3418, .T. ) ;
#11480 = DIRECTION ( 'NONE',  ( 0.000000000000000000, -0.5000000000000008882, 0.8660254037844381525 ) ) ;
#11481 = EDGE_CURVE ( 'NONE', #14342, #9825, #14658, .T. ) ;
#11482 = CARTESIAN_POINT ( 'NONE',  ( -67.59262256747319952, 110.5691553257988460, -26.35917033480641436 ) ) ;
#11483 = ADVANCED_FACE ( 'NONE', ( #13265 ), #7728, .T. ) ;
#11484 = CARTESIAN_POINT ( 'NONE',  ( -49.97371631896665178, 107.0896764944441202, 102.5000000000000000 ) ) ;
#11485 = FACE_OUTER_BOUND ( 'NONE', #3649, .T. ) ;
#11486 = ORIENTED_EDGE ( 'NONE', *, *, #9126, .T. ) ;
#11487 = AXIS2_PLACEMENT_3D ( 'NONE', #14231, #14034, #4203 ) ;
#11488 = LINE ( 'NONE', #3479, #6248 ) ;
#11489 = CARTESIAN_POINT ( 'NONE',  ( -60.18936887439735273, 72.12145385653096241, -167.1454815528550739 ) ) ;
#11490 = DIRECTION ( 'NONE',  ( 1.000000000000000000, 0.000000000000000000, 0.000000000000000000 ) ) ;
#11491 = CARTESIAN_POINT ( 'NONE',  ( -57.08002265617300708, 84.22855780814606419, -124.8487082408420861 ) ) ;
#11492 = ORIENTED_EDGE ( 'NONE', *, *, #5165, .T. ) ;
#11493 = DIRECTION ( 'NONE',  ( -1.000000000000000000, 6.328271240363383445E-14, 1.387778780781443703E-16 ) ) ;
#11494 = DIRECTION ( 'NONE',  ( 0.000000000000000000, 0.000000000000000000, 1.000000000000000000 ) ) ;
#11495 = CARTESIAN_POINT ( 'NONE',  ( -71.24615306438070661, 137.9174286652292096, -15.00000000000001421 ) ) ;
#11496 = ORIENTED_EDGE ( 'NONE', *, *, #8346, .F. ) ;
#11497 = CLOSED_SHELL ( 'NONE', ( #5637, #4901, #11011, #11787, #12967, #9365, #4741, #10084 ) ) ;
#11498 = DIRECTION ( 'NONE',  ( 0.000000000000000000, -1.000000000000000000, 0.000000000000000000 ) ) ;
#11499 = VECTOR ( 'NONE', #10381, 1000.000000000000114 ) ;
#11500 = CYLINDRICAL_SURFACE ( 'NONE', #8082, 42.49926016644946003 ) ;
#11501 = VECTOR ( 'NONE', #13498, 1000.000000000000000 ) ;
#11502 = AXIS2_PLACEMENT_3D ( 'NONE', #1466, #11396, #12892 ) ;
#11503 = CARTESIAN_POINT ( 'NONE',  ( 15.23320273812466041, -19.34983604512934363, -54.79921157549233612 ) ) ;
#11504 = VERTEX_POINT ( 'NONE', #3331 ) ;
#11505 = AXIS2_PLACEMENT_3D ( 'NONE', #16648, #15257, #2555 ) ;
#11506 = EDGE_LOOP ( 'NONE', ( #7960, #6080 ) ) ;
#11507 = EDGE_CURVE ( 'NONE', #9564, #16963, #6129, .T. ) ;
#11508 = CARTESIAN_POINT ( 'NONE',  ( -70.71978124295696944, -96.08423613455721579, 5.204170427930421283E-15 ) ) ;
#11509 = EDGE_LOOP ( 'NONE', ( #437, #7006 ) ) ;
#11510 = DIRECTION ( 'NONE',  ( 0.000000000000000000, 0.000000000000000000, 1.000000000000000000 ) ) ;
#11511 = DIRECTION ( 'NONE',  ( 1.000000000000000000, 0.000000000000000000, 0.000000000000000000 ) ) ;
#11512 = DIRECTION ( 'NONE',  ( 0.000000000000000000, 0.000000000000000000, 1.000000000000000000 ) ) ;
#11513 = CARTESIAN_POINT ( 'NONE',  ( -67.59262256747319952, 111.6514400295689171, -22.50837044127971254 ) ) ;
#11514 = ORIENTED_EDGE ( 'NONE', *, *, #809, .T. ) ;
#11515 = CIRCLE ( 'NONE', #15688, 45.40389983439752086 ) ;
#11516 = DIRECTION ( 'NONE',  ( 0.000000000000000000, 0.000000000000000000, -1.000000000000000000 ) ) ;
#11517 = AXIS2_PLACEMENT_3D ( 'NONE', #12867, #39, #6781 ) ;
#11518 = DIRECTION ( 'NONE',  ( -0.000000000000000000, -0.000000000000000000, 1.000000000000000000 ) ) ;
#11519 = AXIS2_PLACEMENT_3D ( 'NONE', #16537, #648, #3457 ) ;
#11520 = CARTESIAN_POINT ( 'NONE',  ( -68.99615306438094819, 64.84186468813030046, 15.00000000000006928 ) ) ;
#11521 = ORIENTED_EDGE ( 'NONE', *, *, #7501, .F. ) ;
#11522 = CARTESIAN_POINT ( 'NONE',  ( 98.04320049944426785, 84.22855780814606419, 62.50000000000001421 ) ) ;
#11523 = DIRECTION ( 'NONE',  ( 0.000000000000000000, 0.000000000000000000, 1.000000000000000000 ) ) ;
#11524 = ORIENTED_EDGE ( 'NONE', *, *, #15900, .F. ) ;
#11525 = EDGE_CURVE ( 'NONE', #4466, #10176, #1939, .T. ) ;
#11526 = DIRECTION ( 'NONE',  ( 0.9396926207859171987, 0.3420201433256444545, -1.086737899652999999E-16 ) ) ;
#11527 = CARTESIAN_POINT ( 'NONE',  ( -60.71399380653853228, 72.26844686893187486, -167.1454815528550739 ) ) ;
#11528 = ORIENTED_EDGE ( 'NONE', *, *, #12927, .T. ) ;
#11529 = ORIENTED_EDGE ( 'NONE', *, *, #7898, .F. ) ;
#11530 = CIRCLE ( 'NONE', #3431, 5.000000000000004441 ) ;
#11531 = ADVANCED_FACE ( 'NONE', ( #14920 ), #728, .T. ) ;
#11532 = VECTOR ( 'NONE', #15479, 1000.000000000000000 ) ;
#11533 = CARTESIAN_POINT ( 'NONE',  ( -68.12361985383350316, 84.22855780814606419, -62.50000000000000000 ) ) ;
#11534 = DIRECTION ( 'NONE',  ( 0.000000000000000000, 1.000000000000000000, 0.000000000000000000 ) ) ;
#11535 = LINE ( 'NONE', #8718, #18512 ) ;
#11536 = CARTESIAN_POINT ( 'NONE',  ( -47.15582643534892782, 86.78830982163900387, -167.1454815528550739 ) ) ;
#11537 = DIRECTION ( 'NONE',  ( 2.062304371594500494E-16, -1.000000000000000000, 1.073258342404370555E-31 ) ) ;
#11538 = VERTEX_POINT ( 'NONE', #16518 ) ;
#11539 = DIRECTION ( 'NONE',  ( -8.326672684688674053E-15, 0.000000000000000000, 1.000000000000000000 ) ) ;
#11540 = ORIENTED_EDGE ( 'NONE', *, *, #10867, .F. ) ;
#11541 = LINE ( 'NONE', #8727, #1314 ) ;
#11542 = AXIS2_PLACEMENT_3D ( 'NONE', #13446, #6045, #5957 ) ;
#11543 = VECTOR ( 'NONE', #7029, 1000.000000000000000 ) ;
#11544 = DIRECTION ( 'NONE',  ( 0.000000000000000000, -1.000000000000000000, 0.000000000000000000 ) ) ;
#11545 = VERTEX_POINT ( 'NONE', #12328 ) ;
#11546 = ORIENTED_EDGE ( 'NONE', *, *, #3008, .T. ) ;
#11547 = ORIENTED_EDGE ( 'NONE', *, *, #8934, .T. ) ;
#11548 = EDGE_CURVE ( 'NONE', #3566, #13829, #15676, .T. ) ;
#11549 = DIRECTION ( 'NONE',  ( 0.000000000000000000, 0.000000000000000000, -1.000000000000000000 ) ) ;
#11550 = DIRECTION ( 'NONE',  ( 0.000000000000000000, 0.000000000000000000, 1.000000000000000000 ) ) ;
#11551 = DIRECTION ( 'NONE',  ( -1.000000000000000000, -0.000000000000000000, -0.000000000000000000 ) ) ;
#11552 = VERTEX_POINT ( 'NONE', #2392 ) ;
#11553 = ITEM_DEFINED_TRANSFORMATION ( 'NONE', 'NONE', #12362,  #16217 ) ;
#11554 = EDGE_LOOP ( 'NONE', ( #15697, #12324, #7672, #878, #9114 ) ) ;
#11555 = LINE ( 'NONE', #16970, #9298 ) ;
#11556 = DIRECTION ( 'NONE',  ( -1.000000000000000000, -0.000000000000000000, -0.000000000000000000 ) ) ;
#11557 = CARTESIAN_POINT ( 'NONE',  ( -68.99615306438060713, 146.5232735881302517, 15.00000000000006928 ) ) ;
#11558 = VERTEX_POINT ( 'NONE', #12431 ) ;
#11559 = EDGE_CURVE ( 'NONE', #15985, #11213, #6603, .T. ) ;
#11560 = CARTESIAN_POINT ( 'NONE',  ( -68.99615306438077766, 123.9172691816626610, 15.00000000000006928 ) ) ;
#11561 = VERTEX_POINT ( 'NONE', #2498 ) ;
#11562 = EDGE_CURVE ( 'NONE', #6571, #9843, #5103, .T. ) ;
#11563 = ORIENTED_EDGE ( 'NONE', *, *, #3527, .F. ) ;
#11564 = ORIENTED_EDGE ( 'NONE', *, *, #762, .F. ) ;
#11565 = EDGE_CURVE ( 'NONE', #12447, #961, #17436, .T. ) ;
#11566 = EDGE_CURVE ( 'NONE', #14497, #1479, #1914, .T. ) ;
#11567 = CARTESIAN_POINT ( 'NONE',  ( -71.24615306438086293, 90.79353891522923448, 15.00000000000006928 ) ) ;
#11568 = CARTESIAN_POINT ( 'NONE',  ( -46.69442755757756203, 81.24207102880484399, -167.1454815528550739 ) ) ;
#11569 = ORIENTED_EDGE ( 'NONE', *, *, #12149, .T. ) ;
#11570 = CARTESIAN_POINT ( 'NONE',  ( -93.54007869656273044, 187.7866419848965052, -15.00000000000001421 ) ) ;
#11571 = CARTESIAN_POINT ( 'NONE',  ( -68.99615306438083451, 101.9261206316626698, 15.00000000000006928 ) ) ;
#11572 = DIRECTION ( 'NONE',  ( -0.9396926207859008784, 0.3420201433256891965, 1.086737899652981141E-16 ) ) ;
#11573 = DIRECTION ( 'NONE',  ( -0.9396926207859084279, 0.3420201433256686574, 0.000000000000000000 ) ) ;
#11574 = ORIENTED_EDGE ( 'NONE', *, *, #16689, .F. ) ;
#11575 = EDGE_CURVE ( 'NONE', #10909, #14482, #2118, .T. ) ;
#11576 = CARTESIAN_POINT ( 'NONE',  ( -68.99615306438106188, 23.38630438166269698, 15.00000000000006928 ) ) ;
#11577 = EDGE_CURVE ( 'NONE', #16048, #4518, #9326, .T. ) ;
#11578 = CARTESIAN_POINT ( 'NONE',  ( -66.39376235201207521, 88.50596986196454452, 15.00000000000006928 ) ) ;
#11579 = DIRECTION ( 'NONE',  ( 0.000000000000000000, -5.551115123125747573E-17, -1.000000000000000000 ) ) ;
#11580 = EDGE_LOOP ( 'NONE', ( #14047, #12886, #8589, #4651 ) ) ;
#11581 = ADVANCED_FACE ( 'NONE', ( #6707 ), #10643, .T. ) ;
#11582 = CARTESIAN_POINT ( 'NONE',  ( 84.41679105416972106, 84.22855780814606419, 62.50000000000001421 ) ) ;
#11583 = ADVANCED_FACE ( 'NONE', ( #8205 ), #5204, .F. ) ;
#11584 = LINE ( 'NONE', #433, #17632 ) ;
#11585 = VERTEX_POINT ( 'NONE', #13817 ) ;
#11586 = ORIENTED_EDGE ( 'NONE', *, *, #10863, .F. ) ;
#11587 = EDGE_CURVE ( 'NONE', #9725, #13598, #13542, .T. ) ;
#11588 = CARTESIAN_POINT ( 'NONE',  ( 15.23320273812466041, -46.83756720124470263, -115.7605492041889619 ) ) ;
#11589 =( NAMED_UNIT ( * ) SI_UNIT ( $, .STERADIAN. ) SOLID_ANGLE_UNIT ( ) );
#11590 = CARTESIAN_POINT ( 'NONE',  ( -66.28651633149024747, 112.1171927384383764, -25.37060304889219609 ) ) ;
#11591 = DIRECTION ( 'NONE',  ( -0.000000000000000000, -0.000000000000000000, -1.000000000000000000 ) ) ;
#11592 = CARTESIAN_POINT ( 'NONE',  ( -35.03642545851250389, 84.22855780814606419, -61.50000000000000000 ) ) ;
#11593 = ORIENTED_EDGE ( 'NONE', *, *, #7680, .T. ) ;
#11594 = DIRECTION ( 'NONE',  ( 0.9396926207859084279, 0.3420201433256686574, 4.890320548438448905E-16 ) ) ;
#11595 = CARTESIAN_POINT ( 'NONE',  ( -46.95762973216378811, 85.83453492254348305, 15.00000000000006928 ) ) ;
#11596 = DIRECTION ( 'NONE',  ( 0.000000000000000000, 0.000000000000000000, 1.000000000000000000 ) ) ;
#11597 = ORIENTED_EDGE ( 'NONE', *, *, #7030, .F. ) ;
#11598 = CARTESIAN_POINT ( 'NONE',  ( -60.71399380653853228, 72.26844686893187486, -15.00000000000001421 ) ) ;
#11599 = CARTESIAN_POINT ( 'NONE',  ( -107.5926225674731711, 57.88796029049330372, 26.35917033480641436 ) ) ;
#11600 = ORIENTED_EDGE ( 'NONE', *, *, #159, .F. ) ;
#11601 = CARTESIAN_POINT ( 'NONE',  ( -57.56709772515574031, 94.46597735006069740, -15.00000000000001421 ) ) ;
#11602 = CARTESIAN_POINT ( 'NONE',  ( -7.840676406241780860, 112.6569076202650308, 97.49999999999998579 ) ) ;
#11603 = ORIENTED_EDGE ( 'NONE', *, *, #8009, .F. ) ;
#11604 = ORIENTED_EDGE ( 'NONE', *, *, #13499, .F. ) ;
#11605 = AXIS2_PLACEMENT_3D ( 'NONE', #4699, #10415, #14709 ) ;
#11606 = ORIENTED_EDGE ( 'NONE', *, *, #3, .F. ) ;
#11607 = CARTESIAN_POINT ( 'NONE',  ( -71.24615306438070661, 138.8062994045637311, -167.1454815528550739 ) ) ;
#11608 = DIRECTION ( 'NONE',  ( 0.000000000000000000, 0.000000000000000000, 1.000000000000000000 ) ) ;
#11609 = CARTESIAN_POINT ( 'NONE',  ( -123.4618227840623632, -151.5628872026273086, 57.00000000000000000 ) ) ;
#11610 = FACE_OUTER_BOUND ( 'NONE', #18158, .T. ) ;
#11611 = CARTESIAN_POINT ( 'NONE',  ( -68.99615306438100504, 45.37745293166267402, -167.1454815528550739 ) ) ;
#11612 = VERTEX_POINT ( 'NONE', #5007 ) ;
#11613 = DIRECTION ( 'NONE',  ( 1.000000000000000000, 0.000000000000000000, 5.551115123125780730E-16 ) ) ;
#11614 = LINE ( 'NONE', #11445, #3084 ) ;
#11615 = DIRECTION ( 'NONE',  ( 1.000000000000000000, 0.000000000000000000, -0.000000000000000000 ) ) ;
#11616 = VECTOR ( 'NONE', #11254, 1000.000000000000000 ) ;
#11617 = ORIENTED_EDGE ( 'NONE', *, *, #4474, .T. ) ;
#11618 = FACE_OUTER_BOUND ( 'NONE', #18387, .T. ) ;
#11619 = EDGE_LOOP ( 'NONE', ( #13862, #2543, #13224, #17590 ) ) ;
#11620 = ORIENTED_EDGE ( 'NONE', *, *, #8314, .F. ) ;
#11621 = DIRECTION ( 'NONE',  ( -0.000000000000000000, -0.000000000000000000, -1.000000000000000000 ) ) ;
#11622 = PRODUCT_DEFINITION ( 'UNKNOWN', '', #5483, #17679 ) ;
#11623 = VECTOR ( 'NONE', #16798, 1000.000000000000000 ) ;
#11624 = LINE ( 'NONE', #8560, #17438 ) ;
#11625 = CARTESIAN_POINT ( 'NONE',  ( -107.5926225674731853, 110.5691553257988460, 22.35917033480641791 ) ) ;
#11626 = ORIENTED_EDGE ( 'NONE', *, *, #13840, .F. ) ;
#11627 = ORIENTED_EDGE ( 'NONE', *, *, #3196, .T. ) ;
#11628 = CARTESIAN_POINT ( 'NONE',  ( -57.08002265617302839, 27.37185818390810965, 102.5000000000000000 ) ) ;
#11629 = CARTESIAN_POINT ( 'NONE',  ( -57.08002265617300708, 84.22855780814606419, -35.00000000000000000 ) ) ;
#11630 = DIRECTION ( 'NONE',  ( -4.029365176583844474E-15, 0.000000000000000000, 1.000000000000000000 ) ) ;
#11631 = DIRECTION ( 'NONE',  ( -0.9396926207859158664, 0.3420201433256481738, 1.086737899652998397E-16 ) ) ;
#11632 = ORIENTED_EDGE ( 'NONE', *, *, #10166, .T. ) ;
#11633 = CARTESIAN_POINT ( 'NONE',  ( -68.99615306438083451, 101.9261206316626698, -167.1454815528550739 ) ) ;
#11634 = ORIENTED_EDGE ( 'NONE', *, *, #16684, .T. ) ;
#11635 = ADVANCED_FACE ( 'NONE', ( #12222 ), #10722, .T. ) ;
#11636 = ORIENTED_EDGE ( 'NONE', *, *, #376, .F. ) ;
#11637 = VECTOR ( 'NONE', #9874, 1000.000000000000000 ) ;
#11638 = VECTOR ( 'NONE', #3146, 1000.000000000000000 ) ;
#11639 = ORIENTED_EDGE ( 'NONE', *, *, #12398, .F. ) ;
#11640 = FACE_OUTER_BOUND ( 'NONE', #14929, .T. ) ;
#11641 = ADVANCED_FACE ( 'NONE', ( #2213 ), #8098, .F. ) ;
#11642 = FACE_OUTER_BOUND ( 'NONE', #4510, .T. ) ;
#11643 = EDGE_LOOP ( 'NONE', ( #14449, #6344, #17158, #9752, #3471, #388 ) ) ;
#11644 = ADVANCED_FACE ( 'NONE', ( #13638 ), #816, .T. ) ;
#11645 = LINE ( 'NONE', #4528, #13139 ) ;
#11646 = DIRECTION ( 'NONE',  ( -0.000000000000000000, -0.000000000000000000, 1.000000000000000000 ) ) ;
#11647 = DIRECTION ( 'NONE',  ( 0.000000000000000000, 1.000000000000000000, 0.000000000000000000 ) ) ;
#11648 = CONICAL_SURFACE ( 'NONE', #3884, 3.445500000000021767, 0.7853981633974420618 ) ;
#11649 = LINE ( 'NONE', #8940, #18065 ) ;
#11650 = ORIENTED_EDGE ( 'NONE', *, *, #6165, .T. ) ;
#11651 = CARTESIAN_POINT ( 'NONE',  ( -115.7702289486888247, -111.0842361345572158, 5.654315315325360913 ) ) ;
#11652 = AXIS2_PLACEMENT_3D ( 'NONE', #13746, #6632, #17770 ) ;
#11653 = DIRECTION ( 'NONE',  ( -5.204170427930409450E-16, 0.000000000000000000, 1.000000000000000000 ) ) ;
#11654 = DIRECTION ( 'NONE',  ( 0.000000000000000000, 1.000000000000000000, 0.000000000000000000 ) ) ;
#11655 = VERTEX_POINT ( 'NONE', #13920 ) ;
#11656 = EDGE_CURVE ( 'NONE', #11452, #2278, #15498, .T. ) ;
#11657 = EDGE_CURVE ( 'NONE', #15955, #16713, #7594, .T. ) ;
#11658 = CYLINDRICAL_SURFACE ( 'NONE', #18386, 4.599999999999999645 ) ;
#11659 = EDGE_CURVE ( 'NONE', #8947, #15932, #1195, .T. ) ;
#11660 = CARTESIAN_POINT ( 'NONE',  ( -71.24615306438100504, 49.95283446522918780, -15.00000000000001421 ) ) ;
#11661 = ORIENTED_EDGE ( 'NONE', *, *, #8712, .T. ) ;
#11662 = AXIS2_PLACEMENT_3D ( 'NONE', #7383, #13360, #5961 ) ;
#11663 = ORIENTED_EDGE ( 'NONE', *, *, #13405, .F. ) ;
#11665 = ADVANCED_FACE ( 'NONE', ( #12989 ), #9993, .T. ) ;
#11664 = AXIS2_PLACEMENT_3D ( 'NONE', #10180, #4729, #11516 ) ;
#11666 = VECTOR ( 'NONE', #11149, 1000.000000000000000 ) ;
#11667 = EDGE_CURVE ( 'NONE', #5560, #4662, #2790, .T. ) ;
#11668 = CARTESIAN_POINT ( 'NONE',  ( 93.45071565215914688, 84.22855780814606419, 50.20642594383510726 ) ) ;
#11669 = ADVANCED_FACE ( 'NONE', ( #18316 ), #7172, .T. ) ;
#11670 = VERTEX_POINT ( 'NONE', #8299 ) ;
#11671 = CARTESIAN_POINT ( 'NONE',  ( -114.4362239394107377, 110.5691553257988744, -26.35917033480641436 ) ) ;
#11672 =( LENGTH_UNIT ( ) NAMED_UNIT ( * ) SI_UNIT ( .MILLI., .METRE. ) );
#11673 = DIRECTION ( 'NONE',  ( -5.204170427930409450E-16, 0.000000000000000000, 1.000000000000000000 ) ) ;
#11674 = ADVANCED_FACE ( 'NONE', ( #9707 ), #15415, .T. ) ;
#11675 = DIRECTION ( 'NONE',  ( 0.9396926207859084279, 0.3420201433256686574, 0.000000000000000000 ) ) ;
#11676 = ORIENTED_EDGE ( 'NONE', *, *, #7019, .T. ) ;
#11677 = VECTOR ( 'NONE', #14849, 1000.000000000000000 ) ;
#11678 = CARTESIAN_POINT ( 'NONE',  ( -36.03642545851250389, 84.22855780814606419, -61.50000000000000000 ) ) ;
#11679 = LINE ( 'NONE', #17370, #6105 ) ;
#11680 = CYLINDRICAL_SURFACE ( 'NONE', #6744, 10.24899999999999345 ) ;
#11681 = DIRECTION ( 'NONE',  ( -0.9396926207859097602, 0.3420201433256649937, 0.000000000000000000 ) ) ;
#11682 = CONICAL_SURFACE ( 'NONE', #4503, 6.500000000000039968, 1.047197551196600296 ) ;
#11683 = CARTESIAN_POINT ( 'NONE',  ( -37.27023353548769791, 91.32863676353444760, 60.07107215585045878 ) ) ;
#11684 = EDGE_CURVE ( 'NONE', #18359, #6999, #3708, .T. ) ;
#11685 = EDGE_CURVE ( 'NONE', #3670, #11213, #11112, .T. ) ;
#11686 = VECTOR ( 'NONE', #10057, 1000.000000000000000 ) ;
#11687 = EDGE_CURVE ( 'NONE', #315, #13818, #14756, .T. ) ;
#11688 = LINE ( 'NONE', #6049, #6578 ) ;
#11689 = ORIENTED_EDGE ( 'NONE', *, *, #12346, .F. ) ;
#11690 = LINE ( 'NONE', #10559, #11383 ) ;
#11691 = CARTESIAN_POINT ( 'NONE',  ( -57.08002265617300708, 84.22855780814606419, -15.00000000000001421 ) ) ;
#11692 = ORIENTED_EDGE ( 'NONE', *, *, #11910, .F. ) ;
#11693 = ORIENTED_EDGE ( 'NONE', *, *, #14734, .T. ) ;
#11694 = AXIS2_PLACEMENT_3D ( 'NONE', #14350, #17160, #1538 ) ;
#11695 = ORIENTED_EDGE ( 'NONE', *, *, #159, .T. ) ;
#11696 = VECTOR ( 'NONE', #6582, 1000.000000000000000 ) ;
#11697 = AXIS2_PLACEMENT_3D ( 'NONE', #12302, #598, #10514 ) ;
#11698 = EDGE_CURVE ( 'NONE', #10905, #11612, #6998, .T. ) ;
#11699 = DIRECTION ( 'NONE',  ( 1.156482317317869999E-16, 0.000000000000000000, 1.000000000000000000 ) ) ;
#11700 = DIRECTION ( 'NONE',  ( 0.000000000000000000, 0.000000000000000000, 1.000000000000000000 ) ) ;
#11701 = EDGE_CURVE ( 'NONE', #3784, #10995, #10017, .T. ) ;
#11702 = CARTESIAN_POINT ( 'NONE',  ( -66.27474722583565381, 78.55081803573735044, 15.00000000000006928 ) ) ;
#11703 = CARTESIAN_POINT ( 'NONE',  ( -72.85813335477966746, 109.0067719868844449, 22.65648029595582358 ) ) ;
#11704 = CYLINDRICAL_SURFACE ( 'NONE', #12876, 3.999999999999996447 ) ;
#11705 = DIRECTION ( 'NONE',  ( 0.000000000000000000, 1.000000000000000000, -3.330669073875448914E-16 ) ) ;
#11706 = ORIENTED_EDGE ( 'NONE', *, *, #10593, .F. ) ;
#11707 = CARTESIAN_POINT ( 'NONE',  ( -127.5926225674732279, 47.87487112387803023, 15.00000000000004263 ) ) ;
#11708 = CIRCLE ( 'NONE', #644, 10.24900000000000055 ) ;
#11709 = CARTESIAN_POINT ( 'NONE',  ( -81.37409655828280108, -91.08423613455721579, 38.97384619189696764 ) ) ;
#11710 = CARTESIAN_POINT ( 'NONE',  ( -68.99615306438067819, 142.7668250816626596, -167.1454815528550739 ) ) ;
#11711 = VERTEX_POINT ( 'NONE', #14108 ) ;
#11712 = AXIS2_PLACEMENT_3D ( 'NONE', #7606, #13226, #6270 ) ;
#11713 = CARTESIAN_POINT ( 'NONE',  ( -68.99615306438106188, 27.14275288813031040, -167.1454815528550739 ) ) ;
#11714 = VECTOR ( 'NONE', #14949, 1000.000000000000114 ) ;
#11715 = CARTESIAN_POINT ( 'NONE',  ( -57.08002265617300708, 84.22855780814606419, -28.00000000000000355 ) ) ;
#11716 = ORIENTED_EDGE ( 'NONE', *, *, #11575, .F. ) ;
#11717 = VECTOR ( 'NONE', #17092, 1000.000000000000000 ) ;
#11718 = FACE_OUTER_BOUND ( 'NONE', #8707, .T. ) ;
#11719 = PLANE ( 'NONE',  #720 ) ;
#11720 = DIRECTION ( 'NONE',  ( 1.000000000000000000, -0.000000000000000000, -0.000000000000000000 ) ) ;
#11721 = ORIENTED_EDGE ( 'NONE', *, *, #16007, .T. ) ;
#11722 = AXIS2_PLACEMENT_3D ( 'NONE', #12804, #5395, #8212 ) ;
#11723 = CIRCLE ( 'NONE', #12318, 10.24900000000000055 ) ;
#11724 = ORIENTED_EDGE ( 'NONE', *, *, #642, .T. ) ;
#11725 = CYLINDRICAL_SURFACE ( 'NONE', #17657, 45.40389983439752086 ) ;
#11726 = CARTESIAN_POINT ( 'NONE',  ( 7.705628127761821045E-14, -5.948846446049038228, 2.696295709017791253 ) ) ;
#11727 = LINE ( 'NONE', #18419, #4069 ) ;
#11728 = LINE ( 'NONE', #17244, #9946 ) ;
#11729 = ORIENTED_EDGE ( 'NONE', *, *, #5047, .F. ) ;
#11730 = FACE_OUTER_BOUND ( 'NONE', #3252, .T. ) ;
#11731 = VERTEX_POINT ( 'NONE', #2883 ) ;
#11732 = VECTOR ( 'NONE', #2660, 1000.000000000000000 ) ;
#11733 = LINE ( 'NONE', #14217, #13465 ) ;
#11734 = ORIENTED_EDGE ( 'NONE', *, *, #468, .T. ) ;
#11735 = EDGE_CURVE ( 'NONE', #1399, #10391, #434, .T. ) ;
#11736 = AXIS2_PLACEMENT_3D ( 'NONE', #955, #12762, #5624 ) ;
#11737 = VECTOR ( 'NONE', #1451, 1000.000000000000000 ) ;
#11738 = ORIENTED_EDGE ( 'NONE', *, *, #7596, .F. ) ;
#11739 = B_SPLINE_CURVE_WITH_KNOTS ( 'NONE', 3,
 ( #8058, #6468, #6370, #17879, #12286, #16194 ),
 .UNSPECIFIED., .F., .F.,
 ( 4, 2, 4 ),
 ( 0.02294124189247833887, 0.02484059228081024473, 0.02673994266914214712 ),
 .UNSPECIFIED. ) ;
#11740 = DIRECTION ( 'NONE',  ( 1.000000000000000000, 0.000000000000000000, 0.000000000000000000 ) ) ;
#11741 = CARTESIAN_POINT ( 'NONE',  ( -123.4618227840623632, -111.0842361345572158, -7.000000000000013323 ) ) ;
#11742 = AXIS2_PLACEMENT_3D ( 'NONE', #16140, #260, #3242 ) ;
#11743 = ORIENTED_EDGE ( 'NONE', *, *, #7890, .T. ) ;
#11744 = CARTESIAN_POINT ( 'NONE',  ( -57.08002265617300708, 84.22855780814606419, 37.50000000000000000 ) ) ;
#11745 = CARTESIAN_POINT ( 'NONE',  ( -68.99615306438104767, 8.293196988130247860, 15.00000000000006928 ) ) ;
#11746 = CARTESIAN_POINT ( 'NONE',  ( 0.5805565836007609004, -3.752776749732685158, 6.500000000000043521 ) ) ;
#11747 = VERTEX_POINT ( 'NONE', #14289 ) ;
#11748 = CARTESIAN_POINT ( 'NONE',  ( -100.4870060002411805, -151.5628872026273086, -57.00000000000000000 ) ) ;
#11749 = AXIS2_PLACEMENT_3D ( 'NONE', #13263, #10173, #16052 ) ;
#11750 = TOROIDAL_SURFACE ( 'NONE', #3681, 40.40389983439752086, 5.000000000000000000 ) ;
#11751 = CIRCLE ( 'NONE', #4860, 4.600000000000006750 ) ;
#11752 = PLANE ( 'NONE',  #6311 ) ;
#11753 = DIRECTION ( 'NONE',  ( -1.000000000000000000, 0.000000000000000000, 0.000000000000000000 ) ) ;
#11754 = VERTEX_POINT ( 'NONE', #5580 ) ;
#11755 = SPHERICAL_SURFACE ( 'NONE', #16567, 17.12963335357822103 ) ;
#11756 = DIRECTION ( 'NONE',  ( 0.000000000000000000, 0.000000000000000000, 1.000000000000000000 ) ) ;
#11757 = ORIENTED_EDGE ( 'NONE', *, *, #1942, .F. ) ;
#11758 = EDGE_LOOP ( 'NONE', ( #7601, #2905, #4294, #9864 ) ) ;
#11759 = AXIS2_PLACEMENT_3D ( 'NONE', #13349, #16591, #18189 ) ;
#11760 = VECTOR ( 'NONE', #2595, 1000.000000000000000 ) ;
#11761 = AXIS2_PLACEMENT_3D ( 'NONE', #4818, #3421, #7721 ) ;
#11762 = ORIENTED_EDGE ( 'NONE', *, *, #18331, .F. ) ;
#11763 = CARTESIAN_POINT ( 'NONE',  ( -71.24615306438103346, 43.66964916522919538, 15.00000000000006928 ) ) ;
#11764 = ORIENTED_EDGE ( 'NONE', *, *, #6616, .F. ) ;
#11765 = EDGE_CURVE ( 'NONE', #5674, #9250, #1035, .T. ) ;
#11766 = CARTESIAN_POINT ( 'NONE',  ( -66.14901650176582848, 112.1621247781131530, -26.09456109111725652 ) ) ;
#11767 = FACE_OUTER_BOUND ( 'NONE', #8324, .T. ) ;
#11768 = CARTESIAN_POINT ( 'NONE',  ( -107.5926225674731853, 50.58224449241411236, 25.00000000000000000 ) ) ;
#11769 = EDGE_LOOP ( 'NONE', ( #2155, #17525, #14115, #13072 ) ) ;
#11770 = CARTESIAN_POINT ( 'NONE',  ( -102.5926225674731853, 102.8748711238780373, -20.00000000000000355 ) ) ;
#11771 = DIRECTION ( 'NONE',  ( -0.000000000000000000, -0.000000000000000000, -1.000000000000000000 ) ) ;
#11772 = CARTESIAN_POINT ( 'NONE',  ( -69.26024277767963611, 81.41924511788803898, 15.00000000000006928 ) ) ;
#11773 = CARTESIAN_POINT ( 'NONE',  ( -42.53669312409158465, -96.08423613455721579, 5.654315315325685987 ) ) ;
#11774 = CARTESIAN_POINT ( 'NONE',  ( -36.17496312660223623, 86.65089956811803518, 55.39766986458640474 ) ) ;
#11775 = VECTOR ( 'NONE', #6895, 1000.000000000000000 ) ;
#11776 = CIRCLE ( 'NONE', #6698, 12.50000000000001776 ) ;
#11777 = CARTESIAN_POINT ( 'NONE',  ( -57.08002265617300708, 84.22855780814606419, 15.00000000000006928 ) ) ;
#11778 = EDGE_CURVE ( 'NONE', #8597, #15702, #14206, .T. ) ;
#11779 = ORIENTED_EDGE ( 'NONE', *, *, #4452, .F. ) ;
#11780 = ADVANCED_FACE ( 'NONE', ( #15701 ), #13578, .T. ) ;
#11781 = CARTESIAN_POINT ( 'NONE',  ( -66.76897068454591988, 60.14546051432880347, 25.00000000000000355 ) ) ;
#11782 = CARTESIAN_POINT ( 'NONE',  ( -57.08002265617300708, 84.22855780814606419, -15.00000000000001421 ) ) ;
#11783 = ORIENTED_EDGE ( 'NONE', *, *, #1717, .F. ) ;
#11784 = EDGE_LOOP ( 'NONE', ( #18305, #17805, #1422, #1409 ) ) ;
#11785 = CIRCLE ( 'NONE', #8519, 4.600000000000006750 ) ;
#11786 = VECTOR ( 'NONE', #3814, 1000.000000000000000 ) ;
#11787 = ADVANCED_FACE ( 'NONE', ( #64 ), #5762, .T. ) ;
#11788 = VERTEX_POINT ( 'NONE', #16038 ) ;
#11789 = EDGE_CURVE ( 'NONE', #2130, #5246, #14479, .T. ) ;
#11790 = CIRCLE ( 'NONE', #13289, 4.599999999999992539 ) ;
#11791 = EDGE_CURVE ( 'NONE', #15813, #1951, #16253, .T. ) ;
#11792 = VECTOR ( 'NONE', #10566, 1000.000000000000000 ) ;
#11793 = CARTESIAN_POINT ( 'NONE',  ( -215.7064697200939634, 84.22855780814606419, 62.50000000000001421 ) ) ;
#11794 = DIRECTION ( 'NONE',  ( -1.000000000000000000, 0.000000000000000000, 0.000000000000000000 ) ) ;
#11795 = CARTESIAN_POINT ( 'NONE',  ( -76.83302960045048735, 76.97167339262611563, 60.54293804716597549 ) ) ;
#11796 = DIRECTION ( 'NONE',  ( 0.9396926207859043201, 0.3420201433256802037, -1.086737899652985085E-16 ) ) ;
#11797 = EDGE_CURVE ( 'NONE', #16527, #3118, #5930, .T. ) ;
#11798 = DIRECTION ( 'NONE',  ( -1.047634945911800068E-14, 0.000000000000000000, 1.000000000000000000 ) ) ;
#11799 = DIRECTION ( 'NONE',  ( 0.000000000000000000, 0.000000000000000000, -1.000000000000000000 ) ) ;
#11800 = CARTESIAN_POINT ( 'NONE',  ( -92.59262256747321373, 117.8748711238780373, 15.00000000000005862 ) ) ;
#11801 = ORIENTED_EDGE ( 'NONE', *, *, #16710, .T. ) ;
#11802 = EDGE_CURVE ( 'NONE', #17620, #9582, #1761, .T. ) ;
#11803 = AXIS2_PLACEMENT_3D ( 'NONE', #490, #15751, #3282 ) ;
#11804 = CARTESIAN_POINT ( 'NONE',  ( 0.000000000000000000, 0.000000000000000000, 0.000000000000000000 ) ) ;
#11805 = DIRECTION ( 'NONE',  ( 0.000000000000000000, 0.000000000000000000, 1.000000000000000000 ) ) ;
#11806 = CARTESIAN_POINT ( 'NONE',  ( -68.99615306438106188, 30.28434553813027108, -15.00000000000001421 ) ) ;
#11807 = VERTEX_POINT ( 'NONE', #14721 ) ;
#11808 = AXIS2_PLACEMENT_3D ( 'NONE', #3058, #14476, #17448 ) ;
#11809 = CARTESIAN_POINT ( 'NONE',  ( -71.24615306438111872, 18.53690796522925055, -167.1454815528550739 ) ) ;
#11810 = VECTOR ( 'NONE', #18393, 1000.000000000000114 ) ;
#11811 = DIRECTION ( 'NONE',  ( -0.000000000000000000, -0.000000000000000000, 1.000000000000000000 ) ) ;
#11812 = ADVANCED_FACE ( 'NONE', ( #14632 ), #1918, .T. ) ;
#11814 = ORIENTED_EDGE ( 'NONE', *, *, #12242, .T. ) ;
#11813 = VECTOR ( 'NONE', #9822, 1000.000000000000000 ) ;
#11815 = EDGE_CURVE ( 'NONE', #103, #15787, #9032, .T. ) ;
#11816 = ORIENTED_EDGE ( 'NONE', *, *, #2291, .F. ) ;
#11817 = EDGE_CURVE ( 'NONE', #16505, #1922, #11649, .T. ) ;
#11818 = CARTESIAN_POINT ( 'NONE',  ( -71.24615306438100504, 49.95283446522918780, 15.00000000000006928 ) ) ;
#11819 = DIRECTION ( 'NONE',  ( -5.204170427930409450E-16, 0.000000000000000000, 1.000000000000000000 ) ) ;
#11820 = FACE_OUTER_BOUND ( 'NONE', #14026, .T. ) ;
#11821 = EDGE_LOOP ( 'NONE', ( #658, #5087, #17884, #12096, #14504 ) ) ;
#11822=STYLED_ITEM('',(#18538),#12831);
#11823 = VECTOR ( 'NONE', #2986, 1000.000000000000000 ) ;
#11824 = ORIENTED_EDGE ( 'NONE', *, *, #9045, .T. ) ;
#11825 = FACE_OUTER_BOUND ( 'NONE', #13112, .T. ) ;
#11826 = DIRECTION ( 'NONE',  ( 0.000000000000000000, 0.000000000000000000, 1.000000000000000000 ) ) ;
#11827 = LINE ( 'NONE', #17326, #2526 ) ;
#11828 = FACE_OUTER_BOUND ( 'NONE', #12424, .T. ) ;
#11829 = EDGE_LOOP ( 'NONE', ( #5184, #7681, #16456, #9541 ) ) ;
#11830 = CARTESIAN_POINT ( 'NONE',  ( -68.99615306438089135, 67.36860148166267948, -167.1454815528550739 ) ) ;
#11831 = ORIENTED_EDGE ( 'NONE', *, *, #15560, .T. ) ;
#11832 = DIRECTION ( 'NONE',  ( 0.000000000000000000, 0.000000000000000000, 1.000000000000000000 ) ) ;
#11833 = VERTEX_POINT ( 'NONE', #3403 ) ;
#11834 = ORIENTED_EDGE ( 'NONE', *, *, #12840, .F. ) ;
#11835 = DIRECTION ( 'NONE',  ( 1.000000000000000000, -0.000000000000000000, -0.000000000000000000 ) ) ;
#11836 = VERTEX_POINT ( 'NONE', #17260 ) ;
#11837 = DIRECTION ( 'NONE',  ( 0.000000000000000000, 0.000000000000000000, -1.000000000000000000 ) ) ;
#11838 = DIRECTION ( 'NONE',  ( 0.000000000000000000, 0.000000000000000000, -1.000000000000000000 ) ) ;
#11839 = DIRECTION ( 'NONE',  ( 1.156482317317869999E-16, 0.000000000000000000, 1.000000000000000000 ) ) ;
#11840 = ORIENTED_EDGE ( 'NONE', *, *, #6432, .T. ) ;
#11841 = DIRECTION ( 'NONE',  ( -0.000000000000000000, -0.000000000000000000, 1.000000000000000000 ) ) ;
#11842 = DIRECTION ( 'NONE',  ( 0.000000000000000000, 0.000000000000000000, 1.000000000000000000 ) ) ;
#11843 = LINE ( 'NONE', #5769, #14991 ) ;
#11844 = ORIENTED_EDGE ( 'NONE', *, *, #14508, .T. ) ;
#11845 = EDGE_CURVE ( 'NONE', #6867, #1022, #5858, .T. ) ;
#11846 = CARTESIAN_POINT ( 'NONE',  ( -50.78804881079258848, 75.44273092821050852, -167.1454815528550739 ) ) ;
#11847 = LINE ( 'NONE', #17535, #7161 ) ;
#11848 = VERTEX_POINT ( 'NONE', #10515 ) ;
#11849 = EDGE_LOOP ( 'NONE', ( #12289, #18252, #13254, #12189 ) ) ;
#11850 = EDGE_LOOP ( 'NONE', ( #7826, #15013, #2095, #15803 ) ) ;
#11851 = CARTESIAN_POINT ( 'NONE',  ( -47.76080550507955280, 75.89776002577458769, -15.00000000000001421 ) ) ;
#11852 = LINE ( 'NONE', #3513, #10918 ) ;
#11853 = SHAPE_REPRESENTATION_RELATIONSHIP ( 'NONE' , 'NONE' ,  #14258, #13725 ) ;
#11854 = DIRECTION ( 'NONE',  ( 0.000000000000000000, 0.000000000000000000, 1.000000000000000000 ) ) ;
#11855 = CARTESIAN_POINT ( 'NONE',  ( -66.88945454405379110, 81.25920652595873150, -167.1454815528550739 ) ) ;
#11856 = VERTEX_POINT ( 'NONE', #325 ) ;
#11857 = FACE_OUTER_BOUND ( 'NONE', #2946, .T. ) ;
#11858 = DIRECTION ( 'NONE',  ( 0.9396926207859097602, 0.3420201433256649937, 0.000000000000000000 ) ) ;
#11859 = DIRECTION ( 'NONE',  ( -0.9396926207859103153, 0.3420201433256634949, -4.890320548438458766E-16 ) ) ;
#11860 = CARTESIAN_POINT ( 'NONE',  ( 4.699999999999995737, 0.000000000000000000, 0.000000000000000000 ) ) ;
#11861 = CARTESIAN_POINT ( 'NONE',  ( -36.80651802494987379, 89.88064937530403142, 67.45419788538286809 ) ) ;
#11862 = ORIENTED_EDGE ( 'NONE', *, *, #10303, .T. ) ;
#11863 = LINE ( 'NONE', #7465, #2097 ) ;
#11864 = EDGE_LOOP ( 'NONE', ( #10728, #13849, #7708, #89 ) ) ;
#11865 = ADVANCED_FACE ( 'NONE', ( #4709 ), #166, .F. ) ;
#11866 = DIRECTION ( 'NONE',  ( -2.062304371594500494E-16, 1.000000000000000000, 0.000000000000000000 ) ) ;
#11867 = SURFACE_STYLE_USAGE ( .BOTH. , #12060 ) ;
#11868 = ORIENTED_EDGE ( 'NONE', *, *, #7104, .F. ) ;
#11869 = ORIENTED_EDGE ( 'NONE', *, *, #16353, .T. ) ;
#11870 = ORIENTED_EDGE ( 'NONE', *, *, #7863, .F. ) ;
#11871 = CARTESIAN_POINT ( 'NONE',  ( -127.5926225674731995, 110.5691553257988460, -26.35917033480641436 ) ) ;
#11872 = CARTESIAN_POINT ( 'NONE',  ( -102.5926225674731569, 65.58224449241410525, 20.00000000000000355 ) ) ;
#11873 = EDGE_CURVE ( 'NONE', #1167, #10354, #6017, .T. ) ;
#11874 = LINE ( 'NONE', #7924, #16686 ) ;
#11875 = DIRECTION ( 'NONE',  ( 0.000000000000000000, 0.000000000000000000, 1.000000000000000000 ) ) ;
#11876 = DIRECTION ( 'NONE',  ( -0.9396926207859084279, 0.3420201433256686574, 1.086737899652989892E-16 ) ) ;
#11877 = DIRECTION ( 'NONE',  ( 0.000000000000000000, 1.000000000000000000, 0.000000000000000000 ) ) ;
#11878 = CARTESIAN_POINT ( 'NONE',  ( -66.39923980726636898, 75.89776002577445979, 15.00000000000006928 ) ) ;
#11879 = ORIENTED_EDGE ( 'NONE', *, *, #4576, .T. ) ;
#11880 = CARTESIAN_POINT ( 'NONE',  ( -50.06979403241810900, 50.58224449241409104, -26.91246033477409583 ) ) ;
#11881 = CARTESIAN_POINT ( 'NONE',  ( -68.05062368187118693, 78.23723799236674381, -15.00000000000001243 ) ) ;
#11882 = CARTESIAN_POINT ( 'NONE',  ( -68.99615306438083451, 95.64293533166268446, -167.1454815528550739 ) ) ;
#11883 = ORIENTED_EDGE ( 'NONE', *, *, #233, .F. ) ;
#11884 = ADVANCED_FACE ( 'NONE', ( #16213 ), #17528, .T. ) ;
#11885 = EDGE_CURVE ( 'NONE', #17089, #9931, #11203, .T. ) ;
#11886 = DIRECTION ( 'NONE',  ( 0.3420201433256444545, 0.9396926207859171987, -0.000000000000000000 ) ) ;
#11887 = CARTESIAN_POINT ( 'NONE',  ( 0.000000000000000000, 0.000000000000000000, 0.000000000000000000 ) ) ;
#11888 = ORIENTED_EDGE ( 'NONE', *, *, #9835, .F. ) ;
#11889 = AXIS2_PLACEMENT_3D ( 'NONE', #7325, #14436, #15748 ) ;
#11890 = ORIENTED_EDGE ( 'NONE', *, *, #1415, .T. ) ;
#11891 = EDGE_CURVE ( 'NONE', #4210, #10723, #8765, .T. ) ;
#11892 = CARTESIAN_POINT ( 'NONE',  ( -57.08002265617300708, 84.22855780814606419, -167.1454815528550739 ) ) ;
#11893 = EDGE_CURVE ( 'NONE', #12176, #5068, #10248, .T. ) ;
#11894 = CARTESIAN_POINT ( 'NONE',  ( 9.543663295069050534, 56.41207303426870112, -7.000000000000010658 ) ) ;
#11895 = CARTESIAN_POINT ( 'NONE',  ( -71.24615306438086293, 94.82400230456377699, 15.00000000000006928 ) ) ;
#11896 = EDGE_LOOP ( 'NONE', ( #12925, #225, #2765, #6003, #17084, #5350, #15891, #4988, #15582, #7077 ) ) ;
#11897 = EDGE_CURVE ( 'NONE', #18427, #7016, #11790, .T. ) ;
#11898 = DIRECTION ( 'NONE',  ( 0.000000000000000000, 1.000000000000000000, 0.000000000000000000 ) ) ;
#11899 = EDGE_CURVE ( 'NONE', #3150, #3299, #16864, .T. ) ;
#11900 = ORIENTED_EDGE ( 'NONE', *, *, #2908, .F. ) ;
#11901 = AXIS2_PLACEMENT_3D ( 'NONE', #9266, #9184, #13575 ) ;
#11902 = CARTESIAN_POINT ( 'NONE',  ( -47.88529808651028929, 78.55081803573747834, -15.00000000000001421 ) ) ;
#11903 = DIRECTION ( 'NONE',  ( 1.000000000000000000, 0.000000000000000000, 0.000000000000000000 ) ) ;
#11904 = CARTESIAN_POINT ( 'NONE',  ( -51.85133027979232878, 95.58244595420329404, -167.1454815528550739 ) ) ;
#11905 = CARTESIAN_POINT ( 'NONE',  ( -50.78804881079258848, 75.44273092821050852, -15.00000000000001421 ) ) ;
#11906 = VERTEX_POINT ( 'NONE', #3869 ) ;
#11907 = DIRECTION ( 'NONE',  ( 1.000000000000000000, 0.000000000000000000, 0.000000000000000000 ) ) ;
#11908 = EDGE_LOOP ( 'NONE', ( #14618, #3291, #14005, #1679 ) ) ;
#11909 = EDGE_CURVE ( 'NONE', #16431, #162, #143, .T. ) ;
#11910 = EDGE_CURVE ( 'NONE', #4613, #14266, #8075, .T. ) ;
#11911 = DIRECTION ( 'NONE',  ( -1.000000000000000000, 0.000000000000000000, 0.000000000000000000 ) ) ;
#11912 = ORIENTED_EDGE ( 'NONE', *, *, #7535, .F. ) ;
#11913 = ORIENTED_EDGE ( 'NONE', *, *, #12433, .T. ) ;
#11914 = VECTOR ( 'NONE', #12717, 1000.000000000000000 ) ;
#11915 = ORIENTED_EDGE ( 'NONE', *, *, #7014, .T. ) ;
#11916 = FACE_OUTER_BOUND ( 'NONE', #15846, .T. ) ;
#11917 = DIRECTION ( 'NONE',  ( 1.000000000000000000, 0.000000000000000000, 0.000000000000000000 ) ) ;
#11918 = VERTEX_POINT ( 'NONE', #15100 ) ;
#11919 = CARTESIAN_POINT ( 'NONE',  ( -36.03642545851251100, 84.22855780814606419, 55.00000000000001421 ) ) ;
#11920 = EDGE_CURVE ( 'NONE', #7572, #6830, #8806, .T. ) ;
#11921 = CARTESIAN_POINT ( 'NONE',  ( -6.390016554086442547E-15, -0.6346842323188388590, 6.499999999999983125 ) ) ;
#11922 = ORIENTED_EDGE ( 'NONE', *, *, #1512, .F. ) ;
#11923 = DIRECTION ( 'NONE',  ( -0.9396926207859097602, 0.3420201433256649937, 0.000000000000000000 ) ) ;
#11924 = ORIENTED_EDGE ( 'NONE', *, *, #9820, .T. ) ;
#11925 = AXIS2_PLACEMENT_3D ( 'NONE', #17599, #4976, #7883 ) ;
#11926 = DIRECTION ( 'NONE',  ( -1.000000000000000000, 0.000000000000000000, 0.000000000000000000 ) ) ;
#11927 = CARTESIAN_POINT ( 'NONE',  ( -92.59262256747321373, 117.8748711238780373, 35.00000000000000000 ) ) ;
#11928 = ORIENTED_EDGE ( 'NONE', *, *, #1381, .T. ) ;
#11929 = VECTOR ( 'NONE', #18425, 1000.000000000000000 ) ;
#11930 = CARTESIAN_POINT ( 'NONE',  ( -71.24615306438097662, 62.51920506522922949, -167.1454815528550739 ) ) ;
#11931 = CARTESIAN_POINT ( 'NONE',  ( -68.99615306438084872, 93.11619853813030545, -15.00000000000001421 ) ) ;
#11932 = ORIENTED_EDGE ( 'NONE', *, *, #13860, .F. ) ;
#11933 = ORIENTED_EDGE ( 'NONE', *, *, #687, .T. ) ;
#11934 = EDGE_LOOP ( 'NONE', ( #11441, #14971, #16345, #10039, #11274 ) ) ;
#11935 = AXIS2_PLACEMENT_3D ( 'NONE', #10233, #7076, #17166 ) ;
#11936 = DIRECTION ( 'NONE',  ( 0.000000000000000000, 0.000000000000000000, 1.000000000000000000 ) ) ;
#11937 = LINE ( 'NONE', #10715, #706 ) ;
#11938 = VERTEX_POINT ( 'NONE', #17996 ) ;
#11939 = CONICAL_SURFACE ( 'NONE', #10158, 3.999999999999982681, 1.029744258676651203 ) ;
#11940 = APPLICATION_PROTOCOL_DEFINITION ( 'draft international standard', 'automotive_design', 1998, #2503 ) ;
#11941 = PLANE ( 'NONE',  #10614 ) ;
#11942 = DIRECTION ( 'NONE',  ( 0.000000000000000000, 1.000000000000000000, 0.000000000000000000 ) ) ;
#11943 = DIRECTION ( 'NONE',  ( 0.9396926207859084279, 0.3420201433256686574, 0.000000000000000000 ) ) ;
#11944 = ORIENTED_EDGE ( 'NONE', *, *, #5034, .F. ) ;
#11945 = LINE ( 'NONE', #12226, #14367 ) ;
#11946 = PLANE ( 'NONE',  #13927 ) ;
#11947 = CARTESIAN_POINT ( 'NONE',  ( -57.08002265617300708, 84.22855780814606419, -15.00000000000001421 ) ) ;
#11948 = DIRECTION ( 'NONE',  ( -0.000000000000000000, -1.000000000000000000, 0.000000000000000000 ) ) ;
#11949 = CARTESIAN_POINT ( 'NONE',  ( 113.3630170098442989, -111.0842361345572158, 7.000000000000010658 ) ) ;
#11950 = EDGE_LOOP ( 'NONE', ( #6481, #12850, #13060, #2841 ) ) ;
#11951 = DIRECTION ( 'NONE',  ( 1.000000000000000000, 2.062304371594500494E-16, -2.775557561562890858E-16 ) ) ;
#11952 = CARTESIAN_POINT ( 'NONE',  ( -68.99615306438072082, 133.9569029881302811, -15.00000000000001421 ) ) ;
#11953 = EDGE_LOOP ( 'NONE', ( #1429, #3731, #7781, #7417, #9790, #8534 ) ) ;
#11954 = CARTESIAN_POINT ( 'NONE',  ( -66.02602711314098372, 58.23015000473216674, 25.00000000000000355 ) ) ;
#11955 = VECTOR ( 'NONE', #16831, 1000.000000000000000 ) ;
#11956 = VERTEX_POINT ( 'NONE', #5078 ) ;
#11957 = VECTOR ( 'NONE', #9241, 1000.000000000000000 ) ;
#11958 = EDGE_CURVE ( 'NONE', #13900, #16082, #5278, .T. ) ;
#11959 = ORIENTED_EDGE ( 'NONE', *, *, #18323, .T. ) ;
#11960 = AXIS2_PLACEMENT_3D ( 'NONE', #17100, #12501, #879 ) ;
#11961 = VERTEX_POINT ( 'NONE', #2277 ) ;
#11962 = DIRECTION ( 'NONE',  ( 0.000000000000000000, 0.000000000000000000, 1.000000000000000000 ) ) ;
#11963 = CARTESIAN_POINT ( 'NONE',  ( 5.299999999999998934, -3.752776749732685158, 6.500000000000043521 ) ) ;
#11964 = AXIS2_PLACEMENT_3D ( 'NONE', #9925, #2822, #5792 ) ;
#11965 = LINE ( 'NONE', #2046, #17159 ) ;
#11966 = DIRECTION ( 'NONE',  ( -0.9396926207858995461, 0.3420201433256928603, 0.000000000000000000 ) ) ;
#11967 = AXIS2_PLACEMENT_3D ( 'NONE', #15704, #10250, #14635 ) ;
#11968 = LINE ( 'NONE', #17666, #3141 ) ;
#11969 = CARTESIAN_POINT ( 'NONE',  ( -115.7702289486888247, -91.08423613455721579, 5.654315315325360913 ) ) ;
#11970 = VECTOR ( 'NONE', #9313, 1000.000000000000000 ) ;
#11971 = ORIENTED_EDGE ( 'NONE', *, *, #15921, .T. ) ;
#11972 = DIRECTION ( 'NONE',  ( 0.000000000000000000, 0.000000000000000000, 1.000000000000000000 ) ) ;
#11973 = FACE_OUTER_BOUND ( 'NONE', #12883, .T. ) ;
#11974 = LINE ( 'NONE', #8902, #5962 ) ;
#11975 = VERTEX_POINT ( 'NONE', #13418 ) ;
#11976 = CIRCLE ( 'NONE', #3915, 5.000000000000006217 ) ;
#11977 = CARTESIAN_POINT ( 'NONE',  ( -60.06546592763100989, -91.08423613455721579, -28.18308811886527110 ) ) ;
#11978 = CARTESIAN_POINT ( 'NONE',  ( -71.24615306438114715, 13.14259340456377956, -15.00000000000001421 ) ) ;
#11979 = VERTEX_POINT ( 'NONE', #4902 ) ;
#11980 = EDGE_CURVE ( 'NONE', #9028, #12345, #2222, .T. ) ;
#11981 = CIRCLE ( 'NONE', #3921, 47.49926016645014926 ) ;
#11982 = AXIS2_PLACEMENT_3D ( 'NONE', #16592, #3782, #10701 ) ;
#11983 = VERTEX_POINT ( 'NONE', #17808 ) ;
#11984 = CARTESIAN_POINT ( 'NONE',  ( -127.5926225674731711, 57.88796029049329661, 26.35917033480641436 ) ) ;
#11985 = DIRECTION ( 'NONE',  ( 1.000000000000000000, 0.000000000000000000, 4.625929269271485914E-16 ) ) ;
#11986 = LINE ( 'NONE', #3283, #10572 ) ;
#11987 = DIRECTION ( 'NONE',  ( -1.000000000000000000, 6.400974180245392929E-15, 0.000000000000000000 ) ) ;
#11988 = ORIENTED_EDGE ( 'NONE', *, *, #6273, .F. ) ;
#11989 = VECTOR ( 'NONE', #383, 1000.000000000000000 ) ;
#11990 = ADVANCED_FACE ( 'NONE', ( #6683 ), #7983, .F. ) ;
#11991 = DIRECTION ( 'NONE',  ( -5.204170427930409450E-16, 0.000000000000000000, 1.000000000000000000 ) ) ;
#11992 = CARTESIAN_POINT ( 'NONE',  ( -171.0109138863553824, 84.22855780814606419, 70.00000000000001421 ) ) ;
#11993 = ORIENTED_EDGE ( 'NONE', *, *, #16777, .F. ) ;
#11994 = DIRECTION ( 'NONE',  ( 0.000000000000000000, 1.000000000000000000, 0.000000000000000000 ) ) ;
#11995 = CARTESIAN_POINT ( 'NONE',  ( -92.59262256747321373, 110.5691553257988460, -26.35917033480641436 ) ) ;
#11996 = CARTESIAN_POINT ( 'NONE',  ( 0.000000000000000000, 0.000000000000000000, -3.000000000000000000 ) ) ;
#11997 = CARTESIAN_POINT ( 'NONE',  ( -115.7073899772186110, -95.23217669033337529, 5.709860480174842046 ) ) ;
#11998 = VECTOR ( 'NONE', #6225, 1000.000000000000000 ) ;
#11999 = AXIS2_PLACEMENT_3D ( 'NONE', #15820, #5714, #1515 ) ;
#12000 = ORIENTED_EDGE ( 'NONE', *, *, #7126, .F. ) ;
#12001 = LINE ( 'NONE', #16300, #4006 ) ;
#12002 = ORIENTED_EDGE ( 'NONE', *, *, #2182, .F. ) ;
#12003 = EDGE_CURVE ( 'NONE', #13170, #16976, #10798, .T. ) ;
#12004 = CARTESIAN_POINT ( 'NONE',  ( 101.5464244077479492, 84.22855780814606419, 62.50000000000001421 ) ) ;
#12005 = ORIENTED_EDGE ( 'NONE', *, *, #14757, .F. ) ;
#12006 = EDGE_CURVE ( 'NONE', #3050, #1101, #5800, .T. ) ;
#12007 = EDGE_CURVE ( 'NONE', #4073, #8650, #15283, .T. ) ;
#12008 = VECTOR ( 'NONE', #16618, 1000.000000000000000 ) ;
#12009 = VERTEX_POINT ( 'NONE', #10702 ) ;
#12010 = CIRCLE ( 'NONE', #13209, 4.599999999999999645 ) ;
#12011 = VECTOR ( 'NONE', #1128, 1000.000000000000000 ) ;
#12012 = DIRECTION ( 'NONE',  ( 0.000000000000000000, 1.000000000000000000, -0.000000000000000000 ) ) ;
#12013 = CARTESIAN_POINT ( 'NONE',  ( -57.08002265617300708, 84.22855780814606419, 37.50000000000000000 ) ) ;
#12014 = EDGE_CURVE ( 'NONE', #2791, #18427, #18377, .T. ) ;
#12015 = ORIENTED_EDGE ( 'NONE', *, *, #6196, .F. ) ;
#12016 = ADVANCED_FACE ( 'NONE', ( #16494 ), #14768, .T. ) ;
#12017 = ADVANCED_FACE ( 'NONE', ( #2098 ), #14998, .T. ) ;
#12018 = CARTESIAN_POINT ( 'NONE',  ( -68.99615306438089135, 86.83301323813024908, -167.1454815528550739 ) ) ;
#12019 = CARTESIAN_POINT ( 'NONE',  ( -68.99615306438072082, 140.2400882881302948, -167.1454815528550739 ) ) ;
#12020 = VERTEX_POINT ( 'NONE', #3498 ) ;
#12021 = VECTOR ( 'NONE', #5275, 1000.000000000000000 ) ;
#12022 = EDGE_CURVE ( 'NONE', #2924, #16406, #9211, .T. ) ;
#12023 = CARTESIAN_POINT ( 'NONE',  ( -68.30128029835485393, 78.72098330317788850, -15.00000000000001421 ) ) ;
#12024 = ORIENTED_EDGE ( 'NONE', *, *, #13161, .F. ) ;
#12025 = CARTESIAN_POINT ( 'NONE',  ( -68.99615306438094819, 54.80223088166269463, 15.00000000000006928 ) ) ;
#12026 = CARTESIAN_POINT ( 'NONE',  ( -67.59262256747317110, 57.88796029049329661, -26.35917033480641436 ) ) ;
#12027 = EDGE_CURVE ( 'NONE', #1519, #17396, #13518, .T. ) ;
#12028 = CIRCLE ( 'NONE', #6333, 21.04359719766049608 ) ;
#12029 = AXIS2_PLACEMENT_3D ( 'NONE', #2029, #7733, #6322 ) ;
#12030 = CARTESIAN_POINT ( 'NONE',  ( 95.45835937779679625, 56.41207303426869402, -3.000000000000000000 ) ) ;
#12031 = CARTESIAN_POINT ( 'NONE',  ( -76.63889361118792465, -94.42547395655692810, -44.74949031872083083 ) ) ;
#12032 = ORIENTED_EDGE ( 'NONE', *, *, #13485, .T. ) ;
#12033 = ADVANCED_FACE ( 'NONE', ( #13613 ), #6391, .T. ) ;
#12034 = EDGE_CURVE ( 'NONE', #3387, #9128, #17893, .T. ) ;
#12035 = ORIENTED_EDGE ( 'NONE', *, *, #10731, .T. ) ;
#12036 = VECTOR ( 'NONE', #772, 1000.000000000000000 ) ;
#12037 = ORIENTED_EDGE ( 'NONE', *, *, #5247, .F. ) ;
#12038 = FACE_OUTER_BOUND ( 'NONE', #15208, .T. ) ;
#12039 = FACE_OUTER_BOUND ( 'NONE', #6526, .T. ) ;
#12040 = VERTEX_POINT ( 'NONE', #13899 ) ;
#12041 = VECTOR ( 'NONE', #5315, 1000.000000000000000 ) ;
#12042 = CIRCLE ( 'NONE', #10852, 12.49999999999999112 ) ;
#12043 = DIRECTION ( 'NONE',  ( 0.000000000000000000, -5.551115123125747573E-17, -1.000000000000000000 ) ) ;
#12044 = AXIS2_PLACEMENT_3D ( 'NONE', #16435, #10564, #17764 ) ;
#12045 = CARTESIAN_POINT ( 'NONE',  ( -112.5926225674731995, 50.58224449241410525, -15.00000000000000000 ) ) ;
#12046 = DIRECTION ( 'NONE',  ( 1.000000000000000000, 0.000000000000000000, 3.771137991253917233E-16 ) ) ;
#12047 = EDGE_LOOP ( 'NONE', ( #11870, #16190, #4618, #8006 ) ) ;
#12048 = FACE_BOUND ( 'NONE', #12811, .T. ) ;
#12049 = CARTESIAN_POINT ( 'NONE',  ( -70.71978124295696944, -141.5628872026273086, -18.23991632971910803 ) ) ;
#12050 = FACE_OUTER_BOUND ( 'NONE', #5878, .T. ) ;
#12051 = CARTESIAN_POINT ( 'NONE',  ( -12.32444585054070885, 42.03964062063555929, 32.41407232917325132 ) ) ;
#12052 = ORIENTED_EDGE ( 'NONE', *, *, #3879, .T. ) ;
#12053 = AXIS2_PLACEMENT_3D ( 'NONE', #6706, #6602, #18125 ) ;
#12054 = LINE ( 'NONE', #9517, #15062 ) ;
#12055 = CARTESIAN_POINT ( 'NONE',  ( -57.08002265617300708, 84.22855780814606419, 15.00000000000006573 ) ) ;
#12056 = VERTEX_POINT ( 'NONE', #11371 ) ;
#12057 =( GEOMETRIC_REPRESENTATION_CONTEXT ( 3 ) GLOBAL_UNCERTAINTY_ASSIGNED_CONTEXT ( ( #6652 ) ) GLOBAL_UNIT_ASSIGNED_CONTEXT ( ( #6215, #12140, #85 ) ) REPRESENTATION_CONTEXT ( 'NONE', 'WORKASPACE' ) );
#12058 = DIRECTION ( 'NONE',  ( 1.000000000000000000, 0.000000000000000000, -0.000000000000000000 ) ) ;
#12059 = AXIS2_PLACEMENT_3D ( 'NONE', #17204, #17109, #10175 ) ;
#12060 = SURFACE_SIDE_STYLE ('',( #14243 ) ) ;
#12061 = ORIENTED_EDGE ( 'NONE', *, *, #3106, .T. ) ;
#12062 = VECTOR ( 'NONE', #4920, 1000.000000000000227 ) ;
#12063 = VERTEX_POINT ( 'NONE', #12498 ) ;
#12064 = PLANE ( 'NONE',  #12044 ) ;
#12065 = VERTEX_POINT ( 'NONE', #17157 ) ;
#12066 = CARTESIAN_POINT ( 'NONE',  ( -107.5676225674731938, 110.5691553257988460, 26.35917033480641436 ) ) ;
#12067 = CARTESIAN_POINT ( 'NONE',  ( -92.59262256747321373, 110.5691553257988460, -26.35917033480641436 ) ) ;
#12068 = PLANE ( 'NONE',  #12127 ) ;
#12069 = CARTESIAN_POINT ( 'NONE',  ( -65.06546592763127990, -96.08423613455721579, -2.621725226070001387E-13 ) ) ;
#12070 = VECTOR ( 'NONE', #5600, 1000.000000000000000 ) ;
#12071 = DIRECTION ( 'NONE',  ( -1.000000000000000000, 0.000000000000000000, -4.029365176583847629E-15 ) ) ;
#12072 = AXIS2_PLACEMENT_3D ( 'NONE', #1143, #15362, #8340 ) ;
#12073 = CYLINDRICAL_SURFACE ( 'NONE', #3935, 4.599999999999999645 ) ;
#12074 = PRODUCT_DEFINITION_SHAPE ( 'NONE', 'NONE',  #18522 ) ;
#12075 = B_SPLINE_CURVE_WITH_KNOTS ( 'NONE', 3,
 ( #10877, #5062, #861, #17795, #6271, #16380, #8056, #14801, #10494, #3569, #6178, #17594, #4776, #16193, #9287, #3383, #13595, #779, #1991, #6467, #12187, #17878, #2453, #8163, #12387, #16655, #12568, #16751, #5341, #11064, #6762, #13877, #1070, #3948, #13970, #9661, #6848, #964, #12480, #18172, #15370, #10973, #18082, #2563 ),
 .UNSPECIFIED., .F., .F.,
 ( 4, 2, 2, 2, 2, 2, 2, 2, 2, 2, 2, 2, 2, 2, 2, 2, 2, 2, 2, 2, 2, 4 ),
 ( 0.02364448373982101781, 0.02438320150779627049, 0.02512191927577152317, 0.02659935481172202854, 0.02807679034767253390, 0.02955422588362303926, 0.03103166141957354116, 0.03177037918754879731, 0.03250909695552404999, 0.03398653249147452760, 0.03546396802742500520, 0.03694140356337549669, 0.03768012133135077019, 0.03841883909932603675, 0.03915755686730131024, 0.03989627463527657680, 0.04137371017122713768, 0.04285114570717769855, 0.04432858124312825249, 0.04506729901110352599, 0.04580601677907880642, 0.04728345231502940199 ),
 .UNSPECIFIED. ) ;
#12076 = ORIENTED_EDGE ( 'NONE', *, *, #15923, .F. ) ;
#12077 = EDGE_CURVE ( 'NONE', #14173, #1119, #4344, .T. ) ;
#12078 = CARTESIAN_POINT ( 'NONE',  ( -123.4618227840623632, -151.5628872026273086, 57.00000000000000000 ) ) ;
#12079 = LINE ( 'NONE', #10476, #2090 ) ;
#12080 = ORIENTED_EDGE ( 'NONE', *, *, #17376, .T. ) ;
#12081 = MECHANICAL_DESIGN_GEOMETRIC_PRESENTATION_REPRESENTATION (  '', ( #9101 ), #10595 ) ;
#12082 = EDGE_CURVE ( 'NONE', #274, #1231, #6869, .T. ) ;
#12083 = CARTESIAN_POINT ( 'NONE',  ( -25.66933353722516031, -95.65021616327642562, -5.654315315325675328 ) ) ;
#12084 = LINE ( 'NONE', #3551, #13707 ) ;
#12085 = ORIENTED_EDGE ( 'NONE', *, *, #18329, .T. ) ;
#12086 = VECTOR ( 'NONE', #1686, 1000.000000000000000 ) ;
#12087 = ORIENTED_EDGE ( 'NONE', *, *, #5048, .T. ) ;
#12088 = DIRECTION ( 'NONE',  ( 1.000000000000000000, 0.000000000000000000, 0.000000000000000000 ) ) ;
#12089 = CARTESIAN_POINT ( 'NONE',  ( -71.24615306438091977, 79.11603905456372843, -167.1454815528550739 ) ) ;
#12090 = CARTESIAN_POINT ( 'NONE',  ( -71.24615306438097662, 57.12489050456376560, 15.00000000000006928 ) ) ;
#12091 = DIRECTION ( 'NONE',  ( 0.3420201433256686574, 0.9396926207859084279, -0.000000000000000000 ) ) ;
#12092 = VECTOR ( 'NONE', #4506, 1000.000000000000000 ) ;
#12093 = VERTEX_POINT ( 'NONE', #5648 ) ;
#12094 = DIRECTION ( 'NONE',  ( 0.000000000000000000, 0.000000000000000000, 1.000000000000000000 ) ) ;
#12095 = DIRECTION ( 'NONE',  ( -0.000000000000000000, -1.224646799147353207E-16, -1.000000000000000000 ) ) ;
#12096 = ORIENTED_EDGE ( 'NONE', *, *, #4603, .F. ) ;
#12097 = VECTOR ( 'NONE', #10352, 1000.000000000000000 ) ;
#12098 = CARTESIAN_POINT ( 'NONE',  ( 0.4033376246893092820, -4.059728990630953938, -5.968343123267158212 ) ) ;
#12099 = DIRECTION ( 'NONE',  ( -2.775557561562890858E-16, -5.724044492823322765E-32, -1.000000000000000000 ) ) ;
#12100 = DIRECTION ( 'NONE',  ( -0.000000000000000000, 0.000000000000000000, 1.000000000000000000 ) ) ;
#12101 = CARTESIAN_POINT ( 'NONE',  ( -107.5926225674731853, 110.5691553257988460, 26.35917033480641436 ) ) ;
#12102 = TOROIDAL_SURFACE ( 'NONE', #13896, 4.400000000000000355, 0.4000000000000000222 ) ;
#12103 = ORIENTED_EDGE ( 'NONE', *, *, #366, .F. ) ;
#12104 = VECTOR ( 'NONE', #2324, 1000.000000000000000 ) ;
#12105 = DIRECTION ( 'NONE',  ( 0.000000000000000000, 0.000000000000000000, -1.000000000000000000 ) ) ;
#12106 = ORIENTED_EDGE ( 'NONE', *, *, #3204, .F. ) ;
#12107 = DIRECTION ( 'NONE',  ( -1.000000000000000000, -0.000000000000000000, -0.000000000000000000 ) ) ;
#12108 = ORIENTED_EDGE ( 'NONE', *, *, #4360, .T. ) ;
#12109 = ADVANCED_FACE ( 'NONE', ( #9964 ), #7150, .T. ) ;
#12110 = ORIENTED_EDGE ( 'NONE', *, *, #11097, .T. ) ;
#12111 = VECTOR ( 'NONE', #3930, 1000.000000000000114 ) ;
#12112 = VECTOR ( 'NONE', #5108, 1000.000000000000114 ) ;
#12113 = AXIS2_PLACEMENT_3D ( 'NONE', #15979, #1323, #7291 ) ;
#12114 =( LENGTH_UNIT ( ) NAMED_UNIT ( * ) SI_UNIT ( .MILLI., .METRE. ) );
#12115 = CARTESIAN_POINT ( 'NONE',  ( -67.59262256747319952, 110.5691553257988460, 26.35917033480641436 ) ) ;
#12116 = ORIENTED_EDGE ( 'NONE', *, *, #3795, .T. ) ;
#12117 = CARTESIAN_POINT ( 'NONE',  ( -71.24615306438114715, 9.112130015229229940, -15.00000000000001421 ) ) ;
#12118 = EDGE_CURVE ( 'NONE', #70, #18394, #8527, .T. ) ;
#12119 = CARTESIAN_POINT ( 'NONE',  ( -68.99615306438080609, 108.8241617881302545, -167.1454815528550739 ) ) ;
#12120 = EDGE_LOOP ( 'NONE', ( #12344, #1786, #14789, #10959 ) ) ;
#12121 = EDGE_CURVE ( 'NONE', #409, #8399, #14270, .T. ) ;
#12122 = LINE ( 'NONE', #3500, #11406 ) ;
#12123 = VERTEX_POINT ( 'NONE', #11282 ) ;
#12124 = DIRECTION ( 'NONE',  ( -0.9396926207859093161, 0.3420201433256661039, -4.890320548438453836E-16 ) ) ;
#12125 = PLANE ( 'NONE',  #2775 ) ;
#12126 = ORIENTED_EDGE ( 'NONE', *, *, #14327, .T. ) ;
#12127 = AXIS2_PLACEMENT_3D ( 'NONE', #8985, #13371, #8895 ) ;
#12128 = AXIS2_PLACEMENT_3D ( 'NONE', #2169, #7787, #15164 ) ;
#12129 = CARTESIAN_POINT ( 'NONE',  ( -68.99615306438077766, 117.6340838816626899, -15.00000000000001421 ) ) ;
#12130 = ADVANCED_FACE ( 'NONE', ( #15671 ), #8564, .T. ) ;
#12131 = EDGE_CURVE ( 'NONE', #12847, #14807, #1446, .T. ) ;
#12132 = DIRECTION ( 'NONE',  ( 0.000000000000000000, 0.000000000000000000, -1.000000000000000000 ) ) ;
#12133 = ORIENTED_EDGE ( 'NONE', *, *, #9390, .F. ) ;
#12134 = ORIENTED_EDGE ( 'NONE', *, *, #12142, .F. ) ;
#12135 = DIRECTION ( 'NONE',  ( -5.204170427930409450E-16, 0.000000000000000000, 1.000000000000000000 ) ) ;
#12136 = DIRECTION ( 'NONE',  ( 0.3420201433256481738, 0.9396926207859158664, -0.000000000000000000 ) ) ;
#12137 = EDGE_CURVE ( 'NONE', #13598, #11067, #12421, .T. ) ;
#12138 = ORIENTED_EDGE ( 'NONE', *, *, #12927, .F. ) ;
#12139 = CARTESIAN_POINT ( 'NONE',  ( -55.64822083176820655, 96.64628479562776420, -167.1454815528550739 ) ) ;
#12140 =( NAMED_UNIT ( * ) PLANE_ANGLE_UNIT ( ) SI_UNIT ( $, .RADIAN. ) );
#12141 = CARTESIAN_POINT ( 'NONE',  ( 3.411723673005281121, -3.146036035674485642, 51.39613239753626317 ) ) ;
#12142 = EDGE_CURVE ( 'NONE', #9222, #11711, #1171, .T. ) ;
#12143 = CARTESIAN_POINT ( 'NONE',  ( -81.37409655828275845, -91.08423613455721579, 28.18308811886534571 ) ) ;
#12144 = VERTEX_POINT ( 'NONE', #5741 ) ;
#12145 = CARTESIAN_POINT ( 'NONE',  ( -68.99615306438094819, 51.66063823166267355, 15.00000000000006928 ) ) ;
#12146 = CARTESIAN_POINT ( 'NONE',  ( -64.75543355702687620, 94.09456345901884333, -15.00000000000001421 ) ) ;
#12147 = EDGE_CURVE ( 'NONE', #12706, #15989, #2666, .T. ) ;
#12148 = DIRECTION ( 'NONE',  ( 0.000000000000000000, 0.000000000000000000, 1.000000000000000000 ) ) ;
#12149 = EDGE_CURVE ( 'NONE', #17012, #15227, #18085, .T. ) ;
#12150 = DIRECTION ( 'NONE',  ( 1.000000000000000000, 0.000000000000000000, 0.000000000000000000 ) ) ;
#12151 = ORIENTED_EDGE ( 'NONE', *, *, #12240, .F. ) ;
#12152 = CARTESIAN_POINT ( 'NONE',  ( -107.5926225674731853, 110.5691553257988460, -26.35917033480641436 ) ) ;
#12153 = DIRECTION ( 'NONE',  ( 0.000000000000000000, 1.000000000000000000, 0.000000000000000000 ) ) ;
#12154 = ORIENTED_EDGE ( 'NONE', *, *, #11245, .F. ) ;
#12155 = EDGE_CURVE ( 'NONE', #17871, #7519, #10030, .T. ) ;
#12156 = CARTESIAN_POINT ( 'NONE',  ( -57.08002265617300708, 84.22855780814606419, 37.50000000000000000 ) ) ;
#12157 = FILL_AREA_STYLE_COLOUR ( '', #17626 ) ;
#12158 = ORIENTED_EDGE ( 'NONE', *, *, #16810, .F. ) ;
#12159 = ORIENTED_EDGE ( 'NONE', *, *, #15103, .T. ) ;
#12160 = CARTESIAN_POINT ( 'NONE',  ( 103.5381772159376084, -151.5628872026272802, -57.00000000000000000 ) ) ;
#12161 = VERTEX_POINT ( 'NONE', #2859 ) ;
#12162 = CARTESIAN_POINT ( 'NONE',  ( -102.4618227840623774, 0.000000000000000000, 57.00000000000000000 ) ) ;
#12163 = LINE ( 'NONE', #7947, #15325 ) ;
#12164 = DIRECTION ( 'NONE',  ( 0.000000000000000000, -5.551115123125746341E-17, -1.000000000000000000 ) ) ;
#12165 = CARTESIAN_POINT ( 'NONE',  ( -68.99615306438089135, 86.83301323813024908, -167.1454815528550739 ) ) ;
#12166 = CARTESIAN_POINT ( 'NONE',  ( -57.08002265617300708, 84.22855780814606419, 15.00000000000006928 ) ) ;
#12167 = DIRECTION ( 'NONE',  ( 1.000000000000000000, 0.000000000000000000, 0.000000000000000000 ) ) ;
#12168 = VERTEX_POINT ( 'NONE', #8466 ) ;
#12169 = CARTESIAN_POINT ( 'NONE',  ( -73.17959092978806268, 59.66472505855460895, -22.77303213590205644 ) ) ;
#12170 = CARTESIAN_POINT ( 'NONE',  ( -70.71978124295668522, -91.08423613455721579, -17.52877280353970235 ) ) ;
#12171 = EDGE_LOOP ( 'NONE', ( #11003, #10143, #15873, #9869 ) ) ;
#12172 = DIRECTION ( 'NONE',  ( 0.000000000000000000, 1.000000000000000000, 0.000000000000000000 ) ) ;
#12173 = DIRECTION ( 'NONE',  ( 1.156482317317869999E-16, 0.000000000000000000, 1.000000000000000000 ) ) ;
#12174 = ORIENTED_EDGE ( 'NONE', *, *, #11257, .F. ) ;
#12175 = ADVANCED_BREP_SHAPE_REPRESENTATION ( '', ( #84, #16217 ), #15033 ) ;
#12176 = VERTEX_POINT ( 'NONE', #18192 ) ;
#12177 = DIRECTION ( 'NONE',  ( 0.9396926207859093161, 0.3420201433256663814, 4.890320548438453836E-16 ) ) ;
#12178 = CARTESIAN_POINT ( 'NONE',  ( 4.699999999999995737, 0.000000000000000000, 0.000000000000000000 ) ) ;
#12179 = FACE_OUTER_BOUND ( 'NONE', #12120, .T. ) ;
#12180 = DIRECTION ( 'NONE',  ( 0.000000000000000000, 0.000000000000000000, -1.000000000000000000 ) ) ;
#12181 = VERTEX_POINT ( 'NONE', #3965 ) ;
#12182 = LINE ( 'NONE', #959, #12552 ) ;
#12183 = CARTESIAN_POINT ( 'NONE',  ( 1.614557735192997546E-14, 5.469921996229766492, -3.525817189091522863 ) ) ;
#12184 = ORIENTED_EDGE ( 'NONE', *, *, #5402, .F. ) ;
#12185 = CARTESIAN_POINT ( 'NONE',  ( -67.59262256747317110, 56.80567558672318995, -22.50837044127973030 ) ) ;
#12186 = DIRECTION ( 'NONE',  ( -1.000000000000000000, 0.000000000000000000, 1.156482317317869999E-16 ) ) ;
#12187 = CARTESIAN_POINT ( 'NONE',  ( -76.74168354031206718, 91.72869609463793950, 62.00788389762995223 ) ) ;
#12188 = CARTESIAN_POINT ( 'NONE',  ( -92.59262256747321373, 110.5691553257988460, 26.35917033480641436 ) ) ;
#12189 = ORIENTED_EDGE ( 'NONE', *, *, #14542, .F. ) ;
#12190 = CARTESIAN_POINT ( 'NONE',  ( -57.08002265617300708, 84.22855780814606419, 15.00000000000006928 ) ) ;
#12191 = ORIENTED_EDGE ( 'NONE', *, *, #7885, .F. ) ;
#12192 = DIRECTION ( 'NONE',  ( -0.9396926207859069846, 0.3420201433256723766, 0.000000000000000000 ) ) ;
#12193 = ORIENTED_EDGE ( 'NONE', *, *, #828, .T. ) ;
#12194 = EDGE_CURVE ( 'NONE', #12144, #16133, #1264, .T. ) ;
#12195 = EDGE_LOOP ( 'NONE', ( #1379, #17115, #7442, #65, #721, #7677 ) ) ;
#12196 = CARTESIAN_POINT ( 'NONE',  ( -71.24615306438080609, 106.5015021652292404, -167.1454815528550739 ) ) ;
#12197 = CIRCLE ( 'NONE', #4423, 5.000000000000007994 ) ;
#12198 = CYLINDRICAL_SURFACE ( 'NONE', #14136, 10.24900000000001477 ) ;
#12199 = VERTEX_POINT ( 'NONE', #9868 ) ;
#12200 = DIRECTION ( 'NONE',  ( 1.000000000000000000, 2.062304371594500494E-16, -0.000000000000000000 ) ) ;
#12201 = DIRECTION ( 'NONE',  ( -0.9396926207859084279, 0.3420201433256686574, 0.000000000000000000 ) ) ;
#12202 = ORIENTED_EDGE ( 'NONE', *, *, #15561, .T. ) ;
#12203 =( LENGTH_UNIT ( ) NAMED_UNIT ( * ) SI_UNIT ( .MILLI., .METRE. ) );
#12204 = EDGE_CURVE ( 'NONE', #8849, #6958, #14492, .T. ) ;
#12205 = DIRECTION ( 'NONE',  ( 1.000000000000000000, 0.000000000000000000, 0.000000000000000000 ) ) ;
#12206 = ORIENTED_EDGE ( 'NONE', *, *, #12576, .T. ) ;
#12207 = LINE ( 'NONE', #12025, #11132 ) ;
#12208 = FACE_OUTER_BOUND ( 'NONE', #15960, .T. ) ;
#12209 = VERTEX_POINT ( 'NONE', #7070 ) ;
#12210 = FACE_BOUND ( 'NONE', #17933, .T. ) ;
#12211 = CIRCLE ( 'NONE', #3837, 7.500000000000007105 ) ;
#12212 = CARTESIAN_POINT ( 'NONE',  ( -77.34864400865002665, -93.09900722835551790, -43.93281456327065371 ) ) ;
#12213 = ORIENTED_EDGE ( 'NONE', *, *, #2746, .T. ) ;
#12214 = VERTEX_POINT ( 'NONE', #12782 ) ;
#12215 = DIRECTION ( 'NONE',  ( 0.000000000000000000, 0.000000000000000000, 1.000000000000000000 ) ) ;
#12216 = DIRECTION ( 'NONE',  ( 1.000000000000000000, 0.000000000000000000, 0.000000000000000000 ) ) ;
#12217 = VERTEX_POINT ( 'NONE', #18477 ) ;
#12218 = CARTESIAN_POINT ( 'NONE',  ( 5.699999999999996625, 2.678141147339113553E-16, -4.000000000000000000 ) ) ;
#12219 = CARTESIAN_POINT ( 'NONE',  ( -77.62286800010241450, 79.64648582715007308, 56.54243435490922565 ) ) ;
#12220 = CARTESIAN_POINT ( 'NONE',  ( 1.779151955615176695, 2.685460533711434117, 49.75286364766792957 ) ) ;
#12221 = VECTOR ( 'NONE', #15413, 1000.000000000000000 ) ;
#12222 = FACE_OUTER_BOUND ( 'NONE', #145, .T. ) ;
#12223 = ORIENTED_EDGE ( 'NONE', *, *, #9034, .F. ) ;
#12224 = ADVANCED_FACE ( 'NONE', ( #3462 ), #12102, .F. ) ;
#12225 = EDGE_CURVE ( 'NONE', #16358, #18030, #17488, .T. ) ;
#12226 = CARTESIAN_POINT ( 'NONE',  ( 5.299999999999998934, -3.752776749732712691, -6.500000000000033751 ) ) ;
#12227 = CARTESIAN_POINT ( 'NONE',  ( -71.24615306438086293, 88.54081700456373483, -167.1454815528550739 ) ) ;
#12228 = EDGE_CURVE ( 'NONE', #14842, #7034, #652, .T. ) ;
#12229 = LINE ( 'NONE', #10934, #6950 ) ;
#12230 = ORIENTED_EDGE ( 'NONE', *, *, #12608, .T. ) ;
#12231 = CARTESIAN_POINT ( 'NONE',  ( -57.08002265617300708, 84.22855780814606419, -167.1454815528550739 ) ) ;
#12232 = DIRECTION ( 'NONE',  ( -0.9396926207859171987, 0.3420201433256444545, 0.000000000000000000 ) ) ;
#12233 = ORIENTED_EDGE ( 'NONE', *, *, #12953, .T. ) ;
#12234 = DIRECTION ( 'NONE',  ( -0.000000000000000000, -0.000000000000000000, -1.000000000000000000 ) ) ;
#12235 = EDGE_CURVE ( 'NONE', #15896, #6911, #14680, .T. ) ;
#12236 = CARTESIAN_POINT ( 'NONE',  ( -36.62539116635755931, 79.27196096192943742, 68.14973479026978964 ) ) ;
#12237 = ORIENTED_EDGE ( 'NONE', *, *, #13675, .T. ) ;
#12238 = EDGE_CURVE ( 'NONE', #6083, #12209, #17771, .T. ) ;
#12239 = ORIENTED_EDGE ( 'NONE', *, *, #1838, .F. ) ;
#12240 = EDGE_CURVE ( 'NONE', #16069, #2011, #14785, .T. ) ;
#12241 = VECTOR ( 'NONE', #7168, 1000.000000000000000 ) ;
#12242 = EDGE_CURVE ( 'NONE', #797, #11558, #6446, .T. ) ;
#12243 = DIRECTION ( 'NONE',  ( 0.000000000000000000, -0.000000000000000000, -1.000000000000000000 ) ) ;
#12244 = ORIENTED_EDGE ( 'NONE', *, *, #11893, .F. ) ;
#12245 = DIRECTION ( 'NONE',  ( -1.000000000000000000, 0.000000000000000000, 1.692578276882436442E-16 ) ) ;
#12246 = DIRECTION ( 'NONE',  ( 0.3420201433256686574, -0.9396926207859084279, 0.000000000000000000 ) ) ;
#12247 = CARTESIAN_POINT ( 'NONE',  ( -68.99615306438100504, 45.37745293166267402, -15.00000000000001421 ) ) ;
#12248 = EDGE_CURVE ( 'NONE', #13617, #16048, #6342, .T. ) ;
#12249 = ADVANCED_FACE ( 'NONE', ( #9082 ), #10669, .T. ) ;
#12250 = CARTESIAN_POINT ( 'NONE',  ( -57.08002265617300708, 84.22855780814606419, -167.1454815528550739 ) ) ;
#12251 = ADVANCED_FACE ( 'NONE', ( #10471 ), #1774, .T. ) ;
#12252 = CARTESIAN_POINT ( 'NONE',  ( -60.76828531927866095, 74.07097899412299569, -167.1454815528550739 ) ) ;
#12253 = DIRECTION ( 'NONE',  ( -1.000000000000000000, 0.000000000000000000, 0.000000000000000000 ) ) ;
#12254 = CARTESIAN_POINT ( 'NONE',  ( -68.99615306438106188, 24.00116023813026445, 15.00000000000006928 ) ) ;
#12255 = ORIENTED_EDGE ( 'NONE', *, *, #5822, .F. ) ;
#12256 = AXIS2_PLACEMENT_3D ( 'NONE', #12548, #10755, #9741 ) ;
#12257 = EDGE_CURVE ( 'NONE', #9827, #6461, #14860, .T. ) ;
#12258 = CARTESIAN_POINT ( 'NONE',  ( -212.2032458117903104, 94.60860137538374204, 62.50000000000001421 ) ) ;
#12259 = AXIS2_PLACEMENT_3D ( 'NONE', #280, #6151, #7581 ) ;
#12260 = AXIS2_PLACEMENT_3D ( 'NONE', #540, #10373, #17474 ) ;
#12261 = DIRECTION ( 'NONE',  ( 0.000000000000000000, 1.000000000000000000, 0.000000000000000000 ) ) ;
#12262 = ORIENTED_EDGE ( 'NONE', *, *, #5589, .F. ) ;
#12263 = CARTESIAN_POINT ( 'NONE',  ( -68.99615306438100504, 45.37745293166267402, 15.00000000000006928 ) ) ;
#12264 = DIRECTION ( 'NONE',  ( -1.000000000000000000, -1.354062621505947576E-15, 1.692578276882434470E-16 ) ) ;
#12265 = ORIENTED_EDGE ( 'NONE', *, *, #7560, .F. ) ;
#12266 = EDGE_LOOP ( 'NONE', ( #12499, #16307, #16958, #10146 ) ) ;
#12267 = VECTOR ( 'NONE', #12636, 1000.000000000000000 ) ;
#12268 = EDGE_CURVE ( 'NONE', #113, #10347, #8215, .T. ) ;
#12269 = VECTOR ( 'NONE', #10282, 1000.000000000000000 ) ;
#12270 = ADVANCED_FACE ( 'NONE', ( #7753 ), #8825, .T. ) ;
#12271 = EDGE_LOOP ( 'NONE', ( #8548, #7184, #1120, #10855 ) ) ;
#12272 = AXIS2_PLACEMENT_3D ( 'NONE', #7460, #17283, #14660 ) ;
#12273 = CIRCLE ( 'NONE', #12852, 12.29357405616490695 ) ;
#12274 = CARTESIAN_POINT ( 'NONE',  ( -71.24615306438109030, 31.99214930456376038, 15.00000000000006928 ) ) ;
#12275 = LINE ( 'NONE', #13768, #4549 ) ;
#12276 = CARTESIAN_POINT ( 'NONE',  ( -68.99615306438099083, 30.28434553813024621, 15.00000000000006928 ) ) ;
#12277 = LINE ( 'NONE', #9463, #8760 ) ;
#12278 = DIRECTION ( 'NONE',  ( 1.000000000000000000, 0.000000000000000000, -0.000000000000000000 ) ) ;
#12279 = DIRECTION ( 'NONE',  ( 1.000000000000000000, 0.000000000000000000, 0.000000000000000000 ) ) ;
#12280 = ORIENTED_EDGE ( 'NONE', *, *, #6879, .T. ) ;
#12281 = PLANE ( 'NONE',  #18279 ) ;
#12282 = DIRECTION ( 'NONE',  ( 0.000000000000000000, 0.000000000000000000, 1.000000000000000000 ) ) ;
#12284 = EDGE_LOOP ( 'NONE', ( #4167, #13967, #9474, #10394 ) ) ;
#12283 = LINE ( 'NONE', #16571, #12999 ) ;
#12285 = VECTOR ( 'NONE', #6783, 1000.000000000000000 ) ;
#12286 = CARTESIAN_POINT ( 'NONE',  ( 0.4042117618285392400, -3.141900367810186889, -6.500000000000063061 ) ) ;
#12287 = VERTEX_POINT ( 'NONE', #4852 ) ;
#12288 = CARTESIAN_POINT ( 'NONE',  ( -71.24615306438083451, 97.07672421522921979, -15.00000000000001421 ) ) ;
#12289 = ORIENTED_EDGE ( 'NONE', *, *, #15923, .T. ) ;
#12290 = AXIS2_PLACEMENT_3D ( 'NONE', #15394, #15577, #15482 ) ;
#12291 = VECTOR ( 'NONE', #6016, 1000.000000000000000 ) ;
#12292 = PLANE ( 'NONE',  #9817 ) ;
#12293 = ORIENTED_EDGE ( 'NONE', *, *, #12194, .F. ) ;
#12294 = ORIENTED_EDGE ( 'NONE', *, *, #12371, .T. ) ;
#12295 = AXIS2_PLACEMENT_3D ( 'NONE', #908, #284, #8900 ) ;
#12296 = FILL_AREA_STYLE_COLOUR ( '', #4909 ) ;
#12297 = CARTESIAN_POINT ( 'NONE',  ( -71.24615306438091977, 75.08557566522922855, -15.00000000000001421 ) ) ;
#12298 = ORIENTED_EDGE ( 'NONE', *, *, #10291, .F. ) ;
#12299 = APPLICATION_PROTOCOL_DEFINITION ( 'draft international standard', 'automotive_design', 1998, #11001 ) ;
#12300 = VECTOR ( 'NONE', #13497, 1000.000000000000000 ) ;
#12301 = VECTOR ( 'NONE', #5976, 1000.000000000000000 ) ;
#12302 = CARTESIAN_POINT ( 'NONE',  ( -57.08002265617300708, 84.22855780814606419, 37.50000000000000000 ) ) ;
#12303 = CARTESIAN_POINT ( 'NONE',  ( -171.0109138863553824, 84.22855780814606419, 62.50000000000001421 ) ) ;
#12304 = EDGE_LOOP ( 'NONE', ( #5682, #2572 ) ) ;
#12305 = CARTESIAN_POINT ( 'NONE',  ( -50.35400969968294049, 73.69239390902568232, -167.1454815528550739 ) ) ;
#12306 = DIRECTION ( 'NONE',  ( 1.000000000000000000, 0.000000000000000000, 0.000000000000000000 ) ) ;
#12307 = CARTESIAN_POINT ( 'NONE',  ( -68.99615306438118978, -1.131580961869738999, -15.00000000000001421 ) ) ;
#12308 = ORIENTED_EDGE ( 'NONE', *, *, #12514, .F. ) ;
#12309 = CARTESIAN_POINT ( 'NONE',  ( -76.11078808681516250, 106.5972831367397333, -25.83450869657911397 ) ) ;
#12310 = DIRECTION ( 'NONE',  ( -1.000000000000000000, -0.000000000000000000, -0.000000000000000000 ) ) ;
#12312 = ORIENTED_EDGE ( 'NONE', *, *, #9977, .F. ) ;
#12311 = EDGE_CURVE ( 'NONE', #864, #10654, #17766, .T. ) ;
#12313 = CIRCLE ( 'NONE', #1842, 29.36884788726140627 ) ;
#12314 = CARTESIAN_POINT ( 'NONE',  ( -68.99615306438072082, 127.0588618316627105, 15.00000000000006928 ) ) ;
#12315 = EDGE_CURVE ( 'NONE', #17731, #15948, #1971, .T. ) ;
#12316 = CARTESIAN_POINT ( 'NONE',  ( -107.5926225674731995, 60.58224449241411946, -35.00000000000000000 ) ) ;
#12317 = CIRCLE ( 'NONE', #6318, 1.000000000000000888 ) ;
#12318 = AXIS2_PLACEMENT_3D ( 'NONE', #17287, #4470, #2988 ) ;
#12319 = ORIENTED_EDGE ( 'NONE', *, *, #2084, .T. ) ;
#12320 = ORIENTED_EDGE ( 'NONE', *, *, #13958, .T. ) ;
#12321 = CARTESIAN_POINT ( 'NONE',  ( -57.08002265617300708, 84.22855780814606419, -167.1454815528550739 ) ) ;
#12322 = DIRECTION ( 'NONE',  ( -0.000000000000000000, -1.000000000000000000, -0.000000000000000000 ) ) ;
#12323 = VECTOR ( 'NONE', #15931, 1000.000000000000000 ) ;
#12324 = ORIENTED_EDGE ( 'NONE', *, *, #10660, .F. ) ;
#12325 = DIRECTION ( 'NONE',  ( -1.000000000000000000, 0.000000000000000000, 0.000000000000000000 ) ) ;
#12326 = CARTESIAN_POINT ( 'NONE',  ( -77.95601046370802578, 81.56801578385646678, 69.51654028185745915 ) ) ;
#12327 = CARTESIAN_POINT ( 'NONE',  ( -67.32681558843928826, 84.01587117655452630, -15.00000000000001421 ) ) ;
#12328 = CARTESIAN_POINT ( 'NONE',  ( -71.24615306438117557, 2.828944715229236628, -15.00000000000001421 ) ) ;
#12329 = VERTEX_POINT ( 'NONE', #6241 ) ;
#12330 = CARTESIAN_POINT ( 'NONE',  ( -68.99615306438110451, 8.293196988130269176, -15.00000000000001421 ) ) ;
#12331 = AXIS2_PLACEMENT_3D ( 'NONE', #17030, #8253, #2730 ) ;
#12332 = AXIS2_PLACEMENT_3D ( 'NONE', #14274, #3970, #6785 ) ;
#12333 = CARTESIAN_POINT ( 'NONE',  ( 4.699999999999995737, 3.752776749732435135, 6.499999999999981348 ) ) ;
#12334 = DIRECTION ( 'NONE',  ( 0.000000000000000000, 0.000000000000000000, 1.000000000000000000 ) ) ;
#12335 = CARTESIAN_POINT ( 'NONE',  ( -13.50321529758715933, 29.05444879267565739, -39.44013366681765120 ) ) ;
#12336 = CARTESIAN_POINT ( 'NONE',  ( -54.75080917176597950, 94.79374675277695417, 15.00000000000007105 ) ) ;
#12337 = ORIENTED_EDGE ( 'NONE', *, *, #18348, .F. ) ;
#12338 = DIRECTION ( 'NONE',  ( 0.000000000000000000, 0.000000000000000000, 1.000000000000000000 ) ) ;
#12339 = PLANE ( 'NONE',  #10185 ) ;
#12340 = ORIENTED_EDGE ( 'NONE', *, *, #12228, .T. ) ;
#12341 = CIRCLE ( 'NONE', #7561, 12.50000000000000355 ) ;
#12342 = LINE ( 'NONE', #7838, #8065 ) ;
#12343 = CARTESIAN_POINT ( 'NONE',  ( -36.80542140651982663, 78.58944219063717185, 67.45077853189506811 ) ) ;
#12344 = ORIENTED_EDGE ( 'NONE', *, *, #14873, .F. ) ;
#12345 = VERTEX_POINT ( 'NONE', #4955 ) ;
#12346 = EDGE_CURVE ( 'NONE', #16349, #3860, #11968, .T. ) ;
#12347 = AXIS2_PLACEMENT_3D ( 'NONE', #10665, #2045, #3458 ) ;
#12348 = AXIS2_PLACEMENT_3D ( 'NONE', #18153, #5322, #9225 ) ;
#12349 = CARTESIAN_POINT ( 'NONE',  ( -71.24615306438070661, 187.7866419848965052, -167.1454815528550739 ) ) ;
#12350 = ORIENTED_EDGE ( 'NONE', *, *, #17270, .F. ) ;
#12351 = CARTESIAN_POINT ( 'NONE',  ( -66.40868851600845346, 56.38066346224191960, 25.00000000000000355 ) ) ;
#12352 = CARTESIAN_POINT ( 'NONE',  ( -68.99615306438072082, 127.0588618316627105, 15.00000000000006928 ) ) ;
#12353 = DIRECTION ( 'NONE',  ( -0.000000000000000000, 1.000000000000000000, -1.200240087506842815E-16 ) ) ;
#12354 = VECTOR ( 'NONE', #15973, 1000.000000000000000 ) ;
#12355 = DIRECTION ( 'NONE',  ( -0.000000000000000000, -0.000000000000000000, -1.000000000000000000 ) ) ;
#12356 = FACE_OUTER_BOUND ( 'NONE', #11167, .T. ) ;
#12357 = LINE ( 'NONE', #11039, #15621 ) ;
#12358 = VERTEX_POINT ( 'NONE', #16273 ) ;
#12359 = EDGE_CURVE ( 'NONE', #9812, #7225, #3541, .T. ) ;
#12360 = ADVANCED_FACE ( 'NONE', ( #13565 ), #4029, .T. ) ;
#12361 = PLANE ( 'NONE',  #12363 ) ;
#12362 = AXIS2_PLACEMENT_3D ( 'NONE', #1843, #8874, #1748 ) ;
#12363 = AXIS2_PLACEMENT_3D ( 'NONE', #18054, #940, #11042 ) ;
#12364 = AXIS2_PLACEMENT_3D ( 'NONE', #8414, #4016, #18143 ) ;
#12365 = CARTESIAN_POINT ( 'NONE',  ( -97.59262256747321373, 106.8071537307723133, -25.00000000000000000 ) ) ;
#12366 = VERTEX_POINT ( 'NONE', #14037 ) ;
#12367 = DIRECTION ( 'NONE',  ( 0.9396926207859185309, 0.3420201433256406798, 0.000000000000000000 ) ) ;
#12368 = CARTESIAN_POINT ( 'NONE',  ( -92.59262256747318531, 0.3328663868096687350, -25.00000000000000000 ) ) ;
#12369 = EDGE_LOOP ( 'NONE', ( #4431, #4120, #9849, #3496 ) ) ;
#12370 = ORIENTED_EDGE ( 'NONE', *, *, #10358, .F. ) ;
#12371 = EDGE_CURVE ( 'NONE', #9953, #7618, #18241, .T. ) ;
#12372 = ADVANCED_FACE ( 'NONE', ( #12356 ), #5233, .T. ) ;
#12373 = EDGE_CURVE ( 'NONE', #13368, #14342, #3744, .T. ) ;
#12374 = ORIENTED_EDGE ( 'NONE', *, *, #13367, .T. ) ;
#12375 = CIRCLE ( 'NONE', #13257, 6.500000000000039968 ) ;
#12376 = VECTOR ( 'NONE', #10536, 999.9999999999998863 ) ;
#12377 = CYLINDRICAL_SURFACE ( 'NONE', #5000, 3.999999999999989786 ) ;
#12378 = CARTESIAN_POINT ( 'NONE',  ( -70.71978124295696944, -111.0842361345572158, 5.204170427930421283E-15 ) ) ;
#12379 = DIRECTION ( 'NONE',  ( 1.000000000000000000, 0.000000000000000000, 0.000000000000000000 ) ) ;
#12380 = CARTESIAN_POINT ( 'NONE',  ( -68.99615306438089135, 83.69142058813029905, -167.1454815528550739 ) ) ;
#12381 = ADVANCED_FACE ( 'NONE', ( #9634 ), #12544, .T. ) ;
#12382 = LINE ( 'NONE', #1064, #5369 ) ;
#12383 = DIRECTION ( 'NONE',  ( 0.000000000000000000, 0.000000000000000000, -1.000000000000000000 ) ) ;
#12384 = ORIENTED_EDGE ( 'NONE', *, *, #10508, .F. ) ;
#12385 = CARTESIAN_POINT ( 'NONE',  ( -68.99615306438100504, 39.70912348813028103, 15.00000000000006928 ) ) ;
#12386 = PLANE ( 'NONE',  #10496 ) ;
#12388 = ORIENTED_EDGE ( 'NONE', *, *, #7891, .F. ) ;
#12387 = CARTESIAN_POINT ( 'NONE',  ( -76.83752798444122334, 91.47285552305426393, 64.45728441025069344 ) ) ;
#12389 = CARTESIAN_POINT ( 'NONE',  ( -110.0337185876618520, -91.08930958056578220, 10.39386245929412134 ) ) ;
#12390 = ADVANCED_FACE ( 'NONE', ( #11038 ), #6634, .T. ) ;
#12391 = ADVANCED_FACE ( 'NONE', ( #8322 ), #3828, .F. ) ;
#12392 = CARTESIAN_POINT ( 'NONE',  ( 45.30000000000000426, 0.000000000000000000, 0.000000000000000000 ) ) ;
#12393 = ORIENTED_EDGE ( 'NONE', *, *, #4688, .T. ) ;
#12394 = VECTOR ( 'NONE', #4369, 1000.000000000000000 ) ;
#12395 = CARTESIAN_POINT ( 'NONE',  ( -71.24615306438097662, 62.51920506522922949, 15.00000000000006928 ) ) ;
#12397 = ORIENTED_EDGE ( 'NONE', *, *, #2640, .T. ) ;
#12396 = AXIS2_PLACEMENT_3D ( 'NONE', #6085, #11819, #16742 ) ;
#12398 = EDGE_CURVE ( 'NONE', #10161, #14281, #17947, .T. ) ;
#12399 = ORIENTED_EDGE ( 'NONE', *, *, #1955, .F. ) ;
#12400 = DIRECTION ( 'NONE',  ( 0.9396926207859097602, 0.3420201433256649937, -1.086737899652991371E-16 ) ) ;
#12401 = DIRECTION ( 'NONE',  ( 0.9396926207859171987, 0.3420201433256444545, 0.000000000000000000 ) ) ;
#12402 = CARTESIAN_POINT ( 'NONE',  ( 5.233202738124664855, -46.83756720124470263, 115.7605492041889619 ) ) ;
#12403 = VECTOR ( 'NONE', #2609, 1000.000000000000000 ) ;
#12404 = ORIENTED_EDGE ( 'NONE', *, *, #1475, .T. ) ;
#12405 = SHAPE_DEFINITION_REPRESENTATION ( #12710, #8623 ) ;
#12406 = AXIS2_PLACEMENT_3D ( 'NONE', #9777, #6967, #4253 ) ;
#12407 = VECTOR ( 'NONE', #10664, 1000.000000000000000 ) ;
#12408 = LINE ( 'NONE', #6966, #14962 ) ;
#12409 = DIRECTION ( 'NONE',  ( 0.000000000000000000, -5.551115123125747573E-17, -1.000000000000000000 ) ) ;
#12410 = EDGE_LOOP ( 'NONE', ( #14135, #2165, #9536, #12881 ) ) ;
#12411 = SURFACE_STYLE_USAGE ( .BOTH. , #15481 ) ;
#12412 = DIRECTION ( 'NONE',  ( -0.9396926207859158664, 0.3420201433256481738, 1.086737899652998397E-16 ) ) ;
#12413 = CARTESIAN_POINT ( 'NONE',  ( -68.99615306438072082, 130.2004544816626890, 15.00000000000006928 ) ) ;
#12414 = EDGE_LOOP ( 'NONE', ( #148, #15574, #4011, #13315 ) ) ;
#12415 = CARTESIAN_POINT ( 'NONE',  ( -75.72335493167709330, 106.9211863004614997, -28.00000000000000355 ) ) ;
#12416 = DIRECTION ( 'NONE',  ( 0.000000000000000000, 0.000000000000000000, 1.000000000000000000 ) ) ;
#12417 = VERTEX_POINT ( 'NONE', #8235 ) ;
#12418 = DIRECTION ( 'NONE',  ( 0.000000000000000000, 0.000000000000000000, 1.000000000000000000 ) ) ;
#12419 = CIRCLE ( 'NONE', #11235, 7.500000000000007105 ) ;
#12420 = DIRECTION ( 'NONE',  ( 0.000000000000000000, 0.000000000000000000, 1.000000000000000000 ) ) ;
#12421 = CIRCLE ( 'NONE', #11517, 5.000000000000004441 ) ;
#12422 = ORIENTED_EDGE ( 'NONE', *, *, #4359, .T. ) ;
#12423 = AXIS2_PLACEMENT_3D ( 'NONE', #9921, #17435, #14493 ) ;
#12424 = EDGE_LOOP ( 'NONE', ( #10414, #14042, #5653, #13359, #12441, #8722, #5715, #5505, #4382, #4149, #4108, #13634, #10004, #15492, #8638, #15725 ) ) ;
#12425 = DIRECTION ( 'NONE',  ( -0.9396926207859088720, 0.3420201433256675472, 0.000000000000000000 ) ) ;
#12426 = CARTESIAN_POINT ( 'NONE',  ( -71.24615306438091977, 71.94398301522919326, 15.00000000000006928 ) ) ;
#12427 = EDGE_LOOP ( 'NONE', ( #11716, #15732, #18422, #392 ) ) ;
#12428 = CARTESIAN_POINT ( 'NONE',  ( -66.39923980726636898, 75.89776002577445979, -167.1454815528550739 ) ) ;
#12429 = CARTESIAN_POINT ( 'NONE',  ( -78.03761615004539465, 82.26638713947221504, 55.24423648577771218 ) ) ;
#12430 = DIRECTION ( 'NONE',  ( -0.000000000000000000, -0.000000000000000000, -1.000000000000000000 ) ) ;
#12431 = CARTESIAN_POINT ( 'NONE',  ( -68.99615306438072082, 127.6737176881302958, 15.00000000000006928 ) ) ;
#12432 = VERTEX_POINT ( 'NONE', #1219 ) ;
#12433 = EDGE_CURVE ( 'NONE', #10794, #16706, #7914, .T. ) ;
#12434 = DIRECTION ( 'NONE',  ( 0.000000000000000000, 0.000000000000000000, 1.000000000000000000 ) ) ;
#12435 = COLOUR_RGB ( '',0.7921568627450980005, 0.8196078431372548767, 0.9333333333333333481 ) ;
#12436 = DIRECTION ( 'NONE',  ( 0.000000000000000000, -1.000000000000000000, 3.330669073875448914E-16 ) ) ;
#12437 = PLANE ( 'NONE',  #10041 ) ;
#12438 = AXIS2_PLACEMENT_3D ( 'NONE', #10408, #2691, #11630 ) ;
#12439 = LINE ( 'NONE', #15312, #2434 ) ;
#12440 = DIRECTION ( 'NONE',  ( -1.000000000000000000, -0.000000000000000000, -0.000000000000000000 ) ) ;
#12441 = ORIENTED_EDGE ( 'NONE', *, *, #4936, .F. ) ;
#12442 = CARTESIAN_POINT ( 'NONE',  ( 95.45835937779679625, 56.41207303426869402, 7.000000000000010658 ) ) ;
#12443 = CARTESIAN_POINT ( 'NONE',  ( -63.64920489524579494, -92.58099833983884253, 43.41642524957604365 ) ) ;
#12444 = VERTEX_POINT ( 'NONE', #12455 ) ;
#12445 = CARTESIAN_POINT ( 'NONE',  ( -76.06514409945376087, 73.26749283226919829, 97.49999999999998579 ) ) ;
#12446 = CARTESIAN_POINT ( 'NONE',  ( -100.4870060002411805, -151.5628872026273086, -57.00000000000000000 ) ) ;
#12447 = VERTEX_POINT ( 'NONE', #10847 ) ;
#12448 = EDGE_LOOP ( 'NONE', ( #6205, #3162, #10218, #16219 ) ) ;
#12449 = FACE_OUTER_BOUND ( 'NONE', #2357, .T. ) ;
#12450 = ORIENTED_EDGE ( 'NONE', *, *, #7035, .F. ) ;
#12451 = DIRECTION ( 'NONE',  ( 0.000000000000000000, 1.000000000000000000, -5.906678677474559343E-17 ) ) ;
#12452 = FACE_OUTER_BOUND ( 'NONE', #15300, .T. ) ;
#12453 = CARTESIAN_POINT ( 'NONE',  ( 95.45835937779683888, -32.62665103886256190, -3.000000000000000000 ) ) ;
#12454 = CARTESIAN_POINT ( 'NONE',  ( -57.08002265617300708, 84.22855780814606419, 15.00000000000006928 ) ) ;
#12455 = CARTESIAN_POINT ( 'NONE',  ( -61.80899203128051056, 95.79950628479635100, -15.00000000000001421 ) ) ;
#12456 = LINE ( 'NONE', #15524, #17384 ) ;
#12457 = VERTEX_POINT ( 'NONE', #15141 ) ;
#12458 = EDGE_CURVE ( 'NONE', #3309, #885, #10313, .T. ) ;
#12459 = CARTESIAN_POINT ( 'NONE',  ( -71.67320232791250589, 58.72641804341122906, -22.41725278188095061 ) ) ;
#12460 = DIRECTION ( 'NONE',  ( 0.000000000000000000, 0.000000000000000000, 1.000000000000000000 ) ) ;
#12461 = VERTEX_POINT ( 'NONE', #12650 ) ;
#12462 = CARTESIAN_POINT ( 'NONE',  ( -25.66933353722515676, -96.08423613455721579, -5.654315315325675328 ) ) ;
#12463 = DIRECTION ( 'NONE',  ( -5.204170427930409450E-16, 0.000000000000000000, 1.000000000000000000 ) ) ;
#12464 = EDGE_LOOP ( 'NONE', ( #14827, #1913, #8980, #17732 ) ) ;
#12465 = ORIENTED_EDGE ( 'NONE', *, *, #6742, .F. ) ;
#12466 = EDGE_CURVE ( 'NONE', #10167, #8277, #15709, .T. ) ;
#12467 = ORIENTED_EDGE ( 'NONE', *, *, #2350, .F. ) ;
#12468 = UNCERTAINTY_MEASURE_WITH_UNIT (LENGTH_MEASURE( 1.000000000000000082E-05 ), #10446, 'distance_accuracy_value', 'NONE');
#12469 = DIRECTION ( 'NONE',  ( 1.000000000000000000, 1.119176436114069332E-16, 0.000000000000000000 ) ) ;
#12470 = DIRECTION ( 'NONE',  ( 0.000000000000000000, 0.000000000000000000, -1.000000000000000000 ) ) ;
#12471 = CARTESIAN_POINT ( 'NONE',  ( -71.24615306438089135, 82.25763170456374951, 15.00000000000006928 ) ) ;
#12472 = DIRECTION ( 'NONE',  ( -0.000000000000000000, -0.000000000000000000, -1.000000000000000000 ) ) ;
#12473 = DIRECTION ( 'NONE',  ( 0.000000000000000000, 0.000000000000000000, -1.000000000000000000 ) ) ;
#12474 = CARTESIAN_POINT ( 'NONE',  ( -71.24615306438100504, 53.09442711522921599, -167.1454815528550739 ) ) ;
#12475 = CARTESIAN_POINT ( 'NONE',  ( -107.5926225674731853, 102.8748711238780373, -20.00000000000000355 ) ) ;
#12476 = ORIENTED_EDGE ( 'NONE', *, *, #1820, .T. ) ;
#12477 = EDGE_CURVE ( 'NONE', #14712, #8868, #449, .T. ) ;
#12478 = DIRECTION ( 'NONE',  ( 0.000000000000000000, 0.000000000000000000, -1.000000000000000000 ) ) ;
#12479 = LINE ( 'NONE', #1150, #5111 ) ;
#12481 = ORIENTED_EDGE ( 'NONE', *, *, #8337, .T. ) ;
#12480 = CARTESIAN_POINT ( 'NONE',  ( -77.98508218574379214, 86.65089956811806360, 69.60233013541360947 ) ) ;
#12482 = EDGE_CURVE ( 'NONE', #12661, #1399, #7621, .T. ) ;
#12483 = CARTESIAN_POINT ( 'NONE',  ( 5.699999999999996625, 7.830936570423733112E-16, 4.400000000000027889 ) ) ;
#12484 = LINE ( 'NONE', #5263, #1209 ) ;
#12485 = ORIENTED_EDGE ( 'NONE', *, *, #11791, .F. ) ;
#12486 = ADVANCED_FACE ( 'NONE', ( #8133 ), #13847, .T. ) ;
#12487 = DIRECTION ( 'NONE',  ( -0.000000000000000000, 0.000000000000000000, -1.000000000000000000 ) ) ;
#12488 = ORIENTED_EDGE ( 'NONE', *, *, #12034, .F. ) ;
#12489 = EDGE_CURVE ( 'NONE', #6749, #9163, #4643, .T. ) ;
#12490 = ADVANCED_FACE ( 'NONE', ( #5604 ), #11326, .T. ) ;
#12491 = ORIENTED_EDGE ( 'NONE', *, *, #1148, .T. ) ;
#12492 = SURFACE_SIDE_STYLE ('',( #5641 ) ) ;
#12493 = ADVANCED_FACE ( 'NONE', ( #8790 ), #4469, .T. ) ;
#12494 = FACE_OUTER_BOUND ( 'NONE', #1221, .T. ) ;
#12495 = LINE ( 'NONE', #14074, #9035 ) ;
#12496 = EDGE_LOOP ( 'NONE', ( #554, #10283 ) ) ;
#12497 = CARTESIAN_POINT ( 'NONE',  ( -29.41692657362415275, -91.42293623445492301, 8.824457138344833140 ) ) ;
#12498 = CARTESIAN_POINT ( 'NONE',  ( -71.24615306438091977, 75.08557566522922855, 15.00000000000006928 ) ) ;
#12499 = ORIENTED_EDGE ( 'NONE', *, *, #7019, .F. ) ;
#12500 = EDGE_CURVE ( 'NONE', #8524, #12741, #17016, .T. ) ;
#12501 = DIRECTION ( 'NONE',  ( 1.156482317317869999E-16, 0.000000000000000000, 1.000000000000000000 ) ) ;
#12502 = LINE ( 'NONE', #11086, #4223 ) ;
#12503 = EDGE_CURVE ( 'NONE', #18002, #4483, #4208, .T. ) ;
#12504 = CARTESIAN_POINT ( 'NONE',  ( -71.24615306438086293, 90.79353891522923448, -167.1454815528550739 ) ) ;
#12505 = EDGE_LOOP ( 'NONE', ( #3883, #5024 ) ) ;
#12506 = CARTESIAN_POINT ( 'NONE',  ( -86.44887054343442401, 84.22855780814606419, 15.00000000000006573 ) ) ;
#12507 = CYLINDRICAL_SURFACE ( 'NONE', #13526, 7.500000000000007105 ) ;
#12508 = ORIENTED_EDGE ( 'NONE', *, *, #8928, .F. ) ;
#12509 = CARTESIAN_POINT ( 'NONE',  ( -71.24615306438111872, 21.67850061522927518, -15.00000000000001421 ) ) ;
#12510 = CARTESIAN_POINT ( 'NONE',  ( -71.24615306438070661, 137.9174286652292096, 15.00000000000006928 ) ) ;
#12511 = ORIENTED_EDGE ( 'NONE', *, *, #8239, .T. ) ;
#12512 = ORIENTED_EDGE ( 'NONE', *, *, #5725, .T. ) ;
#12513 = VERTEX_POINT ( 'NONE', #4118 ) ;
#12514 = EDGE_CURVE ( 'NONE', #8646, #4482, #15628, .T. ) ;
#12515 = DIRECTION ( 'NONE',  ( 1.000000000000000000, -0.000000000000000000, -0.000000000000000000 ) ) ;
#12516 = FACE_OUTER_BOUND ( 'NONE', #14708, .T. ) ;
#12517 = ORIENTED_EDGE ( 'NONE', *, *, #335, .T. ) ;
#12518 = DIRECTION ( 'NONE',  ( 1.000000000000000000, 0.000000000000000000, 3.771137991253928573E-16 ) ) ;
#12519 = DIRECTION ( 'NONE',  ( 0.9396926207859158664, 0.3420201433256481738, 0.000000000000000000 ) ) ;
#12520 = DIRECTION ( 'NONE',  ( 1.156482317317869999E-16, 0.000000000000000000, 1.000000000000000000 ) ) ;
#12521 = CARTESIAN_POINT ( 'NONE',  ( -68.99615306438100504, 39.09426763166271002, -15.00000000000001421 ) ) ;
#12522 = EDGE_LOOP ( 'NONE', ( #3924, #18469, #8786, #5884 ) ) ;
#12523 = CARTESIAN_POINT ( 'NONE',  ( -68.99615306438120399, -1.131580961869733448, -167.1454815528550739 ) ) ;
#12524 = DIRECTION ( 'NONE',  ( -5.204170427930409450E-16, 0.000000000000000000, 1.000000000000000000 ) ) ;
#12525 = CYLINDRICAL_SURFACE ( 'NONE', #14228, 10.24900000000001477 ) ;
#12526 = VECTOR ( 'NONE', #15810, 1000.000000000000000 ) ;
#12527 = CARTESIAN_POINT ( 'NONE',  ( 2.393365886519067232, 0.7544924491581967985, -50.32767191113995153 ) ) ;
#12528 = DIRECTION ( 'NONE',  ( 0.9396926207859097602, 0.3420201433256649937, 0.000000000000000000 ) ) ;
#12529 = ORIENTED_EDGE ( 'NONE', *, *, #1640, .F. ) ;
#12530 = LINE ( 'NONE', #11225, #17789 ) ;
#12531 = FACE_OUTER_BOUND ( 'NONE', #13740, .T. ) ;
#12532 = PLANE ( 'NONE',  #13458 ) ;
#12533 = CARTESIAN_POINT ( 'NONE',  ( -36.12242916230060530, 82.26638713947218662, 69.75576351422232335 ) ) ;
#12534 = ORIENTED_EDGE ( 'NONE', *, *, #939, .T. ) ;
#12535 = ORIENTED_EDGE ( 'NONE', *, *, #1823, .T. ) ;
#12536 = CIRCLE ( 'NONE', #9525, 12.49999999999999112 ) ;
#12537 = DIRECTION ( 'NONE',  ( 0.000000000000000000, 0.000000000000000000, 1.000000000000000000 ) ) ;
#12538 = DIRECTION ( 'NONE',  ( -1.000000000000000000, -0.000000000000000000, -0.000000000000000000 ) ) ;
#12539 = CARTESIAN_POINT ( 'NONE',  ( -74.91216001386696632, 60.89270028045363858, 23.71611839326908466 ) ) ;
#12540 = CARTESIAN_POINT ( 'NONE',  ( -66.30191238934644105, 56.61994693357914343, 24.99999999999999289 ) ) ;
#12541 = EDGE_LOOP ( 'NONE', ( #7055, #8659, #10835, #7037 ) ) ;
#12542 = DIRECTION ( 'NONE',  ( -1.119176436114069332E-16, 1.000000000000000000, 0.000000000000000000 ) ) ;
#12543 = CARTESIAN_POINT ( 'NONE',  ( -71.24615306438086293, 93.93513156522925556, -15.00000000000001421 ) ) ;
#12544 = CYLINDRICAL_SURFACE ( 'NONE', #9716, 10.24900000000000055 ) ;
#12545 = CARTESIAN_POINT ( 'NONE',  ( -42.53669312409158465, -91.08423613455721579, 10.65431531532568599 ) ) ;
#12546 = ORIENTED_EDGE ( 'NONE', *, *, #8189, .T. ) ;
#12547 = CARTESIAN_POINT ( 'NONE',  ( -71.24615306438114715, 9.112130015229229940, -15.00000000000001421 ) ) ;
#12548 = CARTESIAN_POINT ( 'NONE',  ( -57.08002265617300708, 84.22855780814606419, 37.50000000000000000 ) ) ;
#12549 = ORIENTED_EDGE ( 'NONE', *, *, #12702, .T. ) ;
#12550 = ADVANCED_FACE ( 'NONE', ( #7115 ), #9922, .F. ) ;
#12551 = DIRECTION ( 'NONE',  ( 0.000000000000000000, 1.000000000000000000, 0.000000000000000000 ) ) ;
#12552 = VECTOR ( 'NONE', #6552, 1000.000000000000000 ) ;
#12553 = DIRECTION ( 'NONE',  ( 0.000000000000000000, 0.000000000000000000, 1.000000000000000000 ) ) ;
#12554 = ORIENTED_EDGE ( 'NONE', *, *, #8841, .T. ) ;
#12555 = ORIENTED_EDGE ( 'NONE', *, *, #8477, .F. ) ;
#12556 = ORIENTED_EDGE ( 'NONE', *, *, #10319, .T. ) ;
#12557 = CARTESIAN_POINT ( 'NONE',  ( 4.699999999999995737, -3.752776749732685158, 6.500000000000043521 ) ) ;
#12558 = LINE ( 'NONE', #7049, #12958 ) ;
#12559 = VECTOR ( 'NONE', #15083, 1000.000000000000000 ) ;
#12560 = DIRECTION ( 'NONE',  ( -0.9396926207859084279, 0.3420201433256687684, -4.890320548438449892E-16 ) ) ;
#12561 = LINE ( 'NONE', #10966, #3674 ) ;
#12562 = CARTESIAN_POINT ( 'NONE',  ( 5.233202738124664855, -111.0842361345572158, -57.00000000000000000 ) ) ;
#12563 = VECTOR ( 'NONE', #17132, 1000.000000000000000 ) ;
#12564 = LINE ( 'NONE', #9761, #950 ) ;
#12565 = EDGE_LOOP ( 'NONE', ( #18255, #1049, #16969, #5853 ) ) ;
#12566 = CARTESIAN_POINT ( 'NONE',  ( -31.03642545851250745, 84.22855780814606419, -35.00000000000000711 ) ) ;
#12567 = CARTESIAN_POINT ( 'NONE',  ( -57.08002265617300708, 84.22855780814606419, -167.1454815528550739 ) ) ;
#12569 = ORIENTED_EDGE ( 'NONE', *, *, #14986, .F. ) ;
#12568 = CARTESIAN_POINT ( 'NONE',  ( -76.91954306033080968, 91.24541864506342392, 65.15959670748108579 ) ) ;
#12570 = DIRECTION ( 'NONE',  ( 0.9396926207859171987, 0.3420201433256444545, 0.000000000000000000 ) ) ;
#12571 = DIRECTION ( 'NONE',  ( 0.000000000000000000, 1.000000000000000000, -0.000000000000000000 ) ) ;
#12572 = ORIENTED_EDGE ( 'NONE', *, *, #5835, .F. ) ;
#12573 = DIRECTION ( 'NONE',  ( 0.000000000000000000, 0.000000000000000000, 1.000000000000000000 ) ) ;
#12574 = ORIENTED_EDGE ( 'NONE', *, *, #17850, .T. ) ;
#12575 = VECTOR ( 'NONE', #7564, 1000.000000000000114 ) ;
#12576 = EDGE_CURVE ( 'NONE', #7519, #7091, #10182, .T. ) ;
#12577 = AXIS2_PLACEMENT_3D ( 'NONE', #9829, #1134, #1332 ) ;
#12578 = ORIENTED_EDGE ( 'NONE', *, *, #9755, .F. ) ;
#12579 = ADVANCED_FACE ( 'NONE', ( #13095 ), #4356, .T. ) ;
#12580 = MANIFOLD_SOLID_BREP ( 'Boss-Extrude15[2]', #17430 ) ;
#12581 = PRESENTATION_STYLE_ASSIGNMENT (( #31 ) ) ;
#12582 = CARTESIAN_POINT ( 'NONE',  ( -57.08002265617300708, 84.22855780814606419, -35.00000000000000000 ) ) ;
#12583 = DIRECTION ( 'NONE',  ( -0.9396926207859069846, 0.3420201433256723766, 1.086737899652988166E-16 ) ) ;
#12584 = ORIENTED_EDGE ( 'NONE', *, *, #15356, .F. ) ;
#12585 = SHAPE_DEFINITION_REPRESENTATION ( #18052, #359 ) ;
#12586 =( GEOMETRIC_REPRESENTATION_CONTEXT ( 3 ) GLOBAL_UNCERTAINTY_ASSIGNED_CONTEXT ( ( #665 ) ) GLOBAL_UNIT_ASSIGNED_CONTEXT ( ( #5405, #919, #16625 ) ) REPRESENTATION_CONTEXT ( 'NONE', 'WORKASPACE' ) );
#12587 = ORIENTED_EDGE ( 'NONE', *, *, #3664, .T. ) ;
#12588 = LINE ( 'NONE', #11281, #4799 ) ;
#12589 = VECTOR ( 'NONE', #1474, 1000.000000000000000 ) ;
#12590 = CARTESIAN_POINT ( 'NONE',  ( -107.5926225674732137, 117.8748711238780373, -35.00000000000000000 ) ) ;
#12591 = ORIENTED_EDGE ( 'NONE', *, *, #10651, .F. ) ;
#12592 = LINE ( 'NONE', #16881, #18269 ) ;
#12593 = PLANE ( 'NONE',  #14961 ) ;
#12594 = DIRECTION ( 'NONE',  ( 1.000000000000000000, 0.000000000000000000, 0.000000000000000000 ) ) ;
#12596 = EDGE_CURVE ( 'NONE', #4188, #12009, #8529, .T. ) ;
#12595 = VECTOR ( 'NONE', #90, 1000.000000000000000 ) ;
#12597 = ORIENTED_EDGE ( 'NONE', *, *, #1721, .T. ) ;
#12598 = ADVANCED_FACE ( 'NONE', ( #7292 ), #7732, .T. ) ;
#12599 = CARTESIAN_POINT ( 'NONE',  ( -71.24615306438086293, 93.93513156522925556, -167.1454815528550739 ) ) ;
#12600 = DIRECTION ( 'NONE',  ( -5.204170427930409450E-16, 0.000000000000000000, 1.000000000000000000 ) ) ;
#12601 = ORIENTED_EDGE ( 'NONE', *, *, #3135, .F. ) ;
#12602 = EDGE_CURVE ( 'NONE', #16099, #8042, #3435, .T. ) ;
#12603 = DIRECTION ( 'NONE',  ( 0.000000000000000000, 0.000000000000000000, 1.000000000000000000 ) ) ;
#12604 = AXIS2_PLACEMENT_3D ( 'NONE', #11628, #14179, #18479 ) ;
#12605 = LINE ( 'NONE', #2486, #10585 ) ;
#12606 = VERTEX_POINT ( 'NONE', #14574 ) ;
#12607 = ADVANCED_FACE ( 'NONE', ( #12050 ), #11680, .T. ) ;
#12608 = EDGE_CURVE ( 'NONE', #593, #11376, #6223, .T. ) ;
#12609 = CIRCLE ( 'NONE', #634, 7.500000000000000000 ) ;
#12610 = EDGE_CURVE ( 'NONE', #4147, #8416, #14924, .T. ) ;
#12611 = CIRCLE ( 'NONE', #14665, 3.999999999999989786 ) ;
#12612 = ORIENTED_EDGE ( 'NONE', *, *, #6498, .T. ) ;
#12613 = DIRECTION ( 'NONE',  ( -0.000000000000000000, -0.000000000000000000, -1.000000000000000000 ) ) ;
#12614 = CARTESIAN_POINT ( 'NONE',  ( -123.4618227840623632, -151.5628872026273086, -36.00000000000000000 ) ) ;
#12615 = VERTEX_POINT ( 'NONE', #7831 ) ;
#12616 = EDGE_CURVE ( 'NONE', #7041, #10126, #7635, .T. ) ;
#12617 = DIRECTION ( 'NONE',  ( 0.000000000000000000, 0.000000000000000000, 1.000000000000000000 ) ) ;
#12618 = LINE ( 'NONE', #7088, #14028 ) ;
#12619 = DIRECTION ( 'NONE',  ( 1.000000000000000000, 0.000000000000000000, 0.000000000000000000 ) ) ;
#12620 = CARTESIAN_POINT ( 'NONE',  ( -68.99615306438106188, 35.95267498166268894, -15.00000000000001421 ) ) ;
#12621 = VERTEX_POINT ( 'NONE', #4934 ) ;
#12622 = ADVANCED_FACE ( 'NONE', ( #10646 ), #13356, .F. ) ;
#12623 = VECTOR ( 'NONE', #18265, 1000.000000000000000 ) ;
#12624 = CARTESIAN_POINT ( 'NONE',  ( -64.40194603863702127, 76.28065702765842104, -15.00000000000001421 ) ) ;
#12625 = CARTESIAN_POINT ( 'NONE',  ( -75.02147910882627002, 107.4816543220079410, 23.80484796140106596 ) ) ;
#12626 = DIRECTION ( 'NONE',  ( -0.000000000000000000, -0.000000000000000000, -1.000000000000000000 ) ) ;
#12627 = CARTESIAN_POINT ( 'NONE',  ( -123.4618227840623632, -151.5628872026273086, 57.00000000000000000 ) ) ;
#12628 = ORIENTED_EDGE ( 'NONE', *, *, #5806, .T. ) ;
#12629 = VECTOR ( 'NONE', #7832, 1000.000000000000000 ) ;
#12630 = VECTOR ( 'NONE', #8052, 1000.000000000000000 ) ;
#12631 = EDGE_CURVE ( 'NONE', #18012, #1908, #5241, .T. ) ;
#12632 = LINE ( 'NONE', #1204, #10311 ) ;
#12633 = DIRECTION ( 'NONE',  ( -0.6091372753003161389, 0.7930648017909424086, 0.000000000000000000 ) ) ;
#12634 = EDGE_CURVE ( 'NONE', #13327, #12063, #16058, .T. ) ;
#12635 = LINE ( 'NONE', #9722, #17038 ) ;
#12636 = DIRECTION ( 'NONE',  ( 0.000000000000000000, 0.000000000000000000, 1.000000000000000000 ) ) ;
#12637 = ORIENTED_EDGE ( 'NONE', *, *, #14546, .F. ) ;
#12638 = ORIENTED_EDGE ( 'NONE', *, *, #4199, .F. ) ;
#12639 = VECTOR ( 'NONE', #9121, 1000.000000000000000 ) ;
#12640 = DIRECTION ( 'NONE',  ( 0.9396926207859078728, 0.3420201433256701007, -1.086737899652989152E-16 ) ) ;
#12641 = VERTEX_POINT ( 'NONE', #3519 ) ;
#12642 = AXIS2_PLACEMENT_3D ( 'NONE', #4713, #10081, #17265 ) ;
#12643 = AXIS2_PLACEMENT_3D ( 'NONE', #6224, #11948, #10551 ) ;
#12644 = CARTESIAN_POINT ( 'NONE',  ( -68.99615306438103346, 33.42593818813029571, -15.00000000000001421 ) ) ;
#12645 = DIRECTION ( 'NONE',  ( -0.000000000000000000, -0.000000000000000000, -1.000000000000000000 ) ) ;
#12646 = CARTESIAN_POINT ( 'NONE',  ( -62.67046908522777926, -91.80659809767261947, -42.25010775664318174 ) ) ;
#12647 = ORIENTED_EDGE ( 'NONE', *, *, #3398, .F. ) ;
#12648 = CARTESIAN_POINT ( 'NONE',  ( -66.51364668169603078, 112.0410723289543995, -28.00000000000000355 ) ) ;
#12649 = CARTESIAN_POINT ( 'NONE',  ( 0.4037800551813724992, 7.199367570657603466, 0.5303295852573092217 ) ) ;
#12650 = CARTESIAN_POINT ( 'NONE',  ( -63.34052343625892689, 73.40930968350525632, -15.00000000000001421 ) ) ;
#12651 = CARTESIAN_POINT ( 'NONE',  ( -57.89103256796045116, 73.45256821284057480, -167.1454815528550739 ) ) ;
#12652 = ORIENTED_EDGE ( 'NONE', *, *, #8115, .T. ) ;
#12653 = CIRCLE ( 'NONE', #12940, 5.000000000000000888 ) ;
#12654 = CARTESIAN_POINT ( 'NONE',  ( 5.299999999999998934, 3.752776749732559924, -6.500000000000061284 ) ) ;
#12655 = ORIENTED_EDGE ( 'NONE', *, *, #2972, .F. ) ;
#12656 = AXIS2_PLACEMENT_3D ( 'NONE', #12089, #568, #16286 ) ;
#12657 = LINE ( 'NONE', #11332, #11666 ) ;
#12658 = AXIS2_PLACEMENT_3D ( 'NONE', #4142, #15549, #2646 ) ;
#12659 = PLANE ( 'NONE',  #5027 ) ;
#12660 = VERTEX_POINT ( 'NONE', #16333 ) ;
#12661 = VERTEX_POINT ( 'NONE', #3248 ) ;
#12662 = ORIENTED_EDGE ( 'NONE', *, *, #10666, .F. ) ;
#12663 = VECTOR ( 'NONE', #4553, 1000.000000000000000 ) ;
#12664 = DIRECTION ( 'NONE',  ( 0.000000000000000000, 0.000000000000000000, 1.000000000000000000 ) ) ;
#12665 = DIRECTION ( 'NONE',  ( -4.124608743189000987E-16, 1.000000000000000000, 0.000000000000000000 ) ) ;
#12666 = CARTESIAN_POINT ( 'NONE',  ( -51.34465738200551499, 92.72253132893560235, -15.00000000000001421 ) ) ;
#12667 = EDGE_CURVE ( 'NONE', #11154, #12950, #10550, .T. ) ;
#12668 = VECTOR ( 'NONE', #5229, 1000.000000000000000 ) ;
#12669 = CARTESIAN_POINT ( 'NONE',  ( -92.59262256747319952, 61.64996188551983636, 25.00000000000000000 ) ) ;
#12670 = VECTOR ( 'NONE', #10210, 1000.000000000000000 ) ;
#12671 = VECTOR ( 'NONE', #7546, 1000.000000000000000 ) ;
#12672 = CARTESIAN_POINT ( 'NONE',  ( -68.99615306438086293, 92.50134268166266338, -167.1454815528550739 ) ) ;
#12673 = VERTEX_POINT ( 'NONE', #11772 ) ;
#12674 = DIRECTION ( 'NONE',  ( 0.000000000000000000, 0.000000000000000000, 1.000000000000000000 ) ) ;
#12676 = EDGE_CURVE ( 'NONE', #6428, #5246, #10276, .T. ) ;
#12675 = ORIENTED_EDGE ( 'NONE', *, *, #1800, .F. ) ;
#12677 = CARTESIAN_POINT ( 'NONE',  ( -68.99615306438120399, -1.131580961869733448, -15.00000000000001421 ) ) ;
#12678 = LINE ( 'NONE', #3017, #10751 ) ;
#12679 = EDGE_LOOP ( 'NONE', ( #15767, #8915, #7046, #6651 ) ) ;
#12680 = DIRECTION ( 'NONE',  ( -0.000000000000000000, -0.000000000000000000, -1.000000000000000000 ) ) ;
#12681 = ORIENTED_EDGE ( 'NONE', *, *, #1599, .T. ) ;
#12682 = AXIS2_PLACEMENT_3D ( 'NONE', #10360, #441, #4722 ) ;
#12683 = VECTOR ( 'NONE', #12353, 1000.000000000000000 ) ;
#12684 = AXIS2_PLACEMENT_3D ( 'NONE', #13711, #16322, #17634 ) ;
#12685 = ORIENTED_EDGE ( 'NONE', *, *, #11233, .T. ) ;
#12686 = SURFACE_STYLE_FILL_AREA ( #14072 ) ;
#12687 = CARTESIAN_POINT ( 'NONE',  ( -68.99615306438117557, 5.151604338130305827, -167.1454815528550739 ) ) ;
#12688 = CARTESIAN_POINT ( 'NONE',  ( -46.03642545851250389, 84.22855780814606419, 35.00000000000000000 ) ) ;
#12689 = ORIENTED_EDGE ( 'NONE', *, *, #13066, .T. ) ;
#12690 = CARTESIAN_POINT ( 'NONE',  ( -68.99615306438100504, 49.13390143813029454, -15.00000000000001421 ) ) ;
#12691 = CARTESIAN_POINT ( 'NONE',  ( -68.99615306438087714, 83.69142058813029905, -15.00000000000001421 ) ) ;
#12692 = ORIENTED_EDGE ( 'NONE', *, *, #5939, .T. ) ;
#12693 = DIRECTION ( 'NONE',  ( -5.204170427930409450E-16, 0.000000000000000000, 1.000000000000000000 ) ) ;
#12694 = DIRECTION ( 'NONE',  ( 1.000000000000000000, 2.062304371594500740E-16, -0.000000000000000000 ) ) ;
#12695 = DIRECTION ( 'NONE',  ( 1.000000000000000000, 0.000000000000000000, 0.000000000000000000 ) ) ;
#12696 = VECTOR ( 'NONE', #7457, 1000.000000000000000 ) ;
#12697 = ORIENTED_EDGE ( 'NONE', *, *, #3652, .F. ) ;
#12698 = CIRCLE ( 'NONE', #125, 7.168074330099291736 ) ;
#12699 = CARTESIAN_POINT ( 'NONE',  ( -57.08002265617300708, 84.22855780814606419, -15.00000000000001421 ) ) ;
#12700 = DIRECTION ( 'NONE',  ( -0.000000000000000000, -0.000000000000000000, -1.000000000000000000 ) ) ;
#12701 = EDGE_LOOP ( 'NONE', ( #10036, #11632, #6471, #15788 ) ) ;
#12702 = EDGE_CURVE ( 'NONE', #1661, #6666, #764, .T. ) ;
#12703 = FACE_OUTER_BOUND ( 'NONE', #6175, .T. ) ;
#12704 = AXIS2_PLACEMENT_3D ( 'NONE', #4893, #10615, #16305 ) ;
#12705 = CARTESIAN_POINT ( 'NONE',  ( -66.34462916520553222, 56.35920651190240704, -27.54481102119680003 ) ) ;
#12706 = VERTEX_POINT ( 'NONE', #14661 ) ;
#12707 = VECTOR ( 'NONE', #13450, 1000.000000000000000 ) ;
#12708 = AXIS2_PLACEMENT_3D ( 'NONE', #980, #877, #7807 ) ;
#12709 = VECTOR ( 'NONE', #5, 1000.000000000000000 ) ;
#12710 = PRODUCT_DEFINITION_SHAPE ( 'NONE', 'NONE',  #7481 ) ;
#12711 = ORIENTED_EDGE ( 'NONE', *, *, #2651, .F. ) ;
#12712 = EDGE_CURVE ( 'NONE', #3765, #15435, #356, .T. ) ;
#12713 = LINE ( 'NONE', #5574, #1328 ) ;
#12714 = EDGE_CURVE ( 'NONE', #15151, #6388, #10613, .T. ) ;
#12715 = ORIENTED_EDGE ( 'NONE', *, *, #3907, .F. ) ;
#12716 = LINE ( 'NONE', #18412, #4480 ) ;
#12717 = DIRECTION ( 'NONE',  ( 0.000000000000000000, 1.000000000000000000, 0.000000000000000000 ) ) ;
#12718 = DIRECTION ( 'NONE',  ( 0.000000000000000000, 5.551115123125748189E-17, 1.000000000000000000 ) ) ;
#12719 = DIRECTION ( 'NONE',  ( 1.000000000000000000, 0.000000000000000000, 5.551115123125777772E-16 ) ) ;
#12720 = ORIENTED_EDGE ( 'NONE', *, *, #14331, .T. ) ;
#12721 = CIRCLE ( 'NONE', #9412, 172.7605492041889477 ) ;
#12722 = DIRECTION ( 'NONE',  ( 0.9396926207859158664, 0.3420201433256481738, -1.086737899652998397E-16 ) ) ;
#12723 = DIRECTION ( 'NONE',  ( 0.000000000000000000, 1.000000000000000000, 0.000000000000000000 ) ) ;
#12724 = CARTESIAN_POINT ( 'NONE',  ( -46.69442755757756203, 81.24207102880484399, -15.00000000000001421 ) ) ;
#12725 = DIRECTION ( 'NONE',  ( 0.3420201433256724322, 0.9396926207859070956, -0.000000000000000000 ) ) ;
#12726 = ORIENTED_EDGE ( 'NONE', *, *, #5723, .T. ) ;
#12727 = EDGE_CURVE ( 'NONE', #10691, #11670, #5831, .T. ) ;
#12728 = EDGE_CURVE ( 'NONE', #4389, #2327, #16280, .T. ) ;
#12729 = VECTOR ( 'NONE', #754, 1000.000000000000000 ) ;
#12730 = VECTOR ( 'NONE', #11033, 1000.000000000000000 ) ;
#12731 = CARTESIAN_POINT ( 'NONE',  ( -68.99615306438100504, 48.51904558166270220, -15.00000000000001421 ) ) ;
#12732 = CARTESIAN_POINT ( 'NONE',  ( -68.99615306438072082, 139.6252324316626812, -167.1454815528550739 ) ) ;
#12733 = CARTESIAN_POINT ( 'NONE',  ( 124.5381772159375942, -111.0842361345572158, 7.000000000000010658 ) ) ;
#12734 = DIRECTION ( 'NONE',  ( 0.000000000000000000, 1.000000000000000000, 0.000000000000000000 ) ) ;
#12735 = ORIENTED_EDGE ( 'NONE', *, *, #9610, .F. ) ;
#12736 = ORIENTED_EDGE ( 'NONE', *, *, #10168, .T. ) ;
#12737 = EDGE_CURVE ( 'NONE', #2102, #885, #9061, .T. ) ;
#12738 = EDGE_CURVE ( 'NONE', #4587, #14830, #2605, .T. ) ;
#12739 = LINE ( 'NONE', #8224, #17706 ) ;
#12740 = VECTOR ( 'NONE', #12603, 1000.000000000000000 ) ;
#12741 = VERTEX_POINT ( 'NONE', #16522 ) ;
#12742 = VECTOR ( 'NONE', #1853, 1000.000000000000000 ) ;
#12743 = ADVANCED_FACE ( 'NONE', ( #733 ), #18027, .T. ) ;
#12744 = VECTOR ( 'NONE', #10018, 1000.000000000000000 ) ;
#12745 = DIRECTION ( 'NONE',  ( -0.000000000000000000, -0.000000000000000000, -1.000000000000000000 ) ) ;
#12746 = CARTESIAN_POINT ( 'NONE',  ( -102.5926225674731569, 65.58224449241410525, 20.00000000000000355 ) ) ;
#12747 = EDGE_CURVE ( 'NONE', #8708, #5168, #11118, .T. ) ;
#12748 = CARTESIAN_POINT ( 'NONE',  ( -61.37143594624207310, -91.24992749556382421, -40.65007029793605398 ) ) ;
#12749 = VERTEX_POINT ( 'NONE', #6608 ) ;
#12750 = CARTESIAN_POINT ( 'NONE',  ( -71.24615306438103346, 43.66964916522919538, -15.00000000000001421 ) ) ;
#12751 = CARTESIAN_POINT ( 'NONE',  ( -71.24615306438091977, 79.11603905456372843, 15.00000000000006928 ) ) ;
#12752 = DIRECTION ( 'NONE',  ( 0.000000000000000000, -5.551115123125747573E-17, -1.000000000000000000 ) ) ;
#12753 = ORIENTED_EDGE ( 'NONE', *, *, #9174, .T. ) ;
#12754 = ADVANCED_FACE ( 'NONE', ( #6805 ), #12437, .T. ) ;
#12755 = LINE ( 'NONE', #14040, #2406 ) ;
#12756 = ORIENTED_EDGE ( 'NONE', *, *, #17315, .F. ) ;
#12757 = LINE ( 'NONE', #101, #261 ) ;
#12758 = EDGE_LOOP ( 'NONE', ( #10140, #16214, #2757, #4821 ) ) ;
#12759 = ORIENTED_EDGE ( 'NONE', *, *, #10190, .F. ) ;
#12760 = EDGE_LOOP ( 'NONE', ( #14507, #4218, #8017, #9636, #10292, #18290 ) ) ;
#12761 = CARTESIAN_POINT ( 'NONE',  ( -46.03642545851250389, 84.22855780814606419, 37.50000000000000000 ) ) ;
#12762 = DIRECTION ( 'NONE',  ( 1.156482317317869999E-16, 0.000000000000000000, 1.000000000000000000 ) ) ;
#12763 = DIRECTION ( 'NONE',  ( -1.119176436114069332E-16, 1.000000000000000000, 0.000000000000000000 ) ) ;
#12764 = DIRECTION ( 'NONE',  ( -0.000000000000000000, -1.000000000000000000, -0.000000000000000000 ) ) ;
#12765 = DIRECTION ( 'NONE',  ( 1.000000000000000000, 0.000000000000000000, 0.000000000000000000 ) ) ;
#12766 = ORIENTED_EDGE ( 'NONE', *, *, #5712, .F. ) ;
#12767 = CARTESIAN_POINT ( 'NONE',  ( -47.27059076829218043, 81.25920652595885940, -15.00000000000001421 ) ) ;
#12768 = ORIENTED_EDGE ( 'NONE', *, *, #14584, .F. ) ;
#12769 = CARTESIAN_POINT ( 'NONE',  ( -68.99615306438091977, 77.40823528813029952, -15.00000000000001421 ) ) ;
#12770 = FACE_OUTER_BOUND ( 'NONE', #4734, .T. ) ;
#12771 = ORIENTED_EDGE ( 'NONE', *, *, #16401, .T. ) ;
#12772 = DIRECTION ( 'NONE',  ( -5.204170427930409450E-16, 0.000000000000000000, 1.000000000000000000 ) ) ;
#12773 = ORIENTED_EDGE ( 'NONE', *, *, #18187, .F. ) ;
#12774 = ORIENTED_EDGE ( 'NONE', *, *, #1271, .F. ) ;
#12775 = LINE ( 'NONE', #9673, #15383 ) ;
#12776 = LINE ( 'NONE', #17056, #10281 ) ;
#12777 = DIRECTION ( 'NONE',  ( -0.5150380749100562650, 1.049727191138617217E-16, -0.8571673007021111124 ) ) ;
#12778 = ORIENTED_EDGE ( 'NONE', *, *, #10534, .F. ) ;
#12779 = CONTEXT_DEPENDENT_SHAPE_REPRESENTATION ( #2378, #3543 ) ;
#12780 = ORIENTED_EDGE ( 'NONE', *, *, #11100, .F. ) ;
#12781 = CARTESIAN_POINT ( 'NONE',  ( -32.62048503522395038, 55.23029653342705814, -23.63796962397022838 ) ) ;
#12782 = CARTESIAN_POINT ( 'NONE',  ( -61.80899203128051056, 95.79950628479635100, 15.00000000000006928 ) ) ;
#12783 = VERTEX_POINT ( 'NONE', #8103 ) ;
#12784 = LINE ( 'NONE', #4513, #7799 ) ;
#12785 = FACE_OUTER_BOUND ( 'NONE', #12496, .T. ) ;
#12786 = DIRECTION ( 'NONE',  ( -0.000000000000000000, -0.000000000000000000, -1.000000000000000000 ) ) ;
#12787 = ORIENTED_EDGE ( 'NONE', *, *, #11071, .F. ) ;
#12788 = CARTESIAN_POINT ( 'NONE',  ( -102.5926225674731000, -8.980688996350953114E-14, 0.000000000000000000 ) ) ;
#12789 = ORIENTED_EDGE ( 'NONE', *, *, #6404, .T. ) ;
#12790 = VERTEX_POINT ( 'NONE', #10931 ) ;
#12791 = EDGE_CURVE ( 'NONE', #7041, #538, #821, .T. ) ;
#12792 = CARTESIAN_POINT ( 'NONE',  ( -100.4870060002411805, -151.5628872026273086, -57.00000000000000000 ) ) ;
#12793 = ORIENTED_EDGE ( 'NONE', *, *, #5866, .T. ) ;
#12794 = LINE ( 'NONE', #11297, #9676 ) ;
#12795 = LINE ( 'NONE', #12614, #11760 ) ;
#12796 = ORIENTED_EDGE ( 'NONE', *, *, #2784, .F. ) ;
#12797 = CARTESIAN_POINT ( 'NONE',  ( -47.59681378869034774, 80.34130291867735707, -167.1454815528550739 ) ) ;
#12798 = CARTESIAN_POINT ( 'NONE',  ( -57.08002265617300708, 84.22855780814606419, -15.00000000000001421 ) ) ;
#12799 = CARTESIAN_POINT ( 'NONE',  ( 49.38736944425944841, -141.5628872026273086, 57.00000000000000000 ) ) ;
#12800 = CARTESIAN_POINT ( 'NONE',  ( -68.99615306438079188, 93.11619853813027703, 15.00000000000006928 ) ) ;
#12801 = ORIENTED_EDGE ( 'NONE', *, *, #16664, .F. ) ;
#12802 = PLANE ( 'NONE',  #312 ) ;
#12803 = LINE ( 'NONE', #5672, #11717 ) ;
#12804 = CARTESIAN_POINT ( 'NONE',  ( -68.99615306438106188, 36.56753083813027416, -167.1454815528550739 ) ) ;
#12805 = ORIENTED_EDGE ( 'NONE', *, *, #3418, .F. ) ;
#12806 = LINE ( 'NONE', #2798, #12403 ) ;
#12807 = PLANE ( 'NONE',  #3595 ) ;
#12808 = CARTESIAN_POINT ( 'NONE',  ( -57.08002265617302839, 27.37185818390810965, 102.5000000000000000 ) ) ;
#12809 = FACE_OUTER_BOUND ( 'NONE', #4102, .T. ) ;
#12810 = EDGE_LOOP ( 'NONE', ( #6953, #17835, #9117, #4634 ) ) ;
#12811 = EDGE_LOOP ( 'NONE', ( #1910, #15856 ) ) ;
#12812 = LINE ( 'NONE', #14029, #1005 ) ;
#12813 = ORIENTED_EDGE ( 'NONE', *, *, #12118, .T. ) ;
#12814 = ADVANCED_FACE ( 'NONE', ( #6508 ), #3612, .T. ) ;
#12815 = FACE_OUTER_BOUND ( 'NONE', #15296, .T. ) ;
#12816 = VECTOR ( 'NONE', #15469, 1000.000000000000000 ) ;
#12817 = CARTESIAN_POINT ( 'NONE',  ( -64.65314733921357515, -94.06000665574431707, -44.58117175117413211 ) ) ;
#12818 = ADVANCED_FACE ( 'NONE', ( #2305 ), #12525, .T. ) ;
#12819 = ORIENTED_EDGE ( 'NONE', *, *, #15441, .T. ) ;
#12820 = CARTESIAN_POINT ( 'NONE',  ( -71.24615306438103346, 44.55851990456372391, 15.00000000000006928 ) ) ;
#12821 = DIRECTION ( 'NONE',  ( -0.000000000000000000, -1.000000000000000000, -0.000000000000000000 ) ) ;
#12822 = DIRECTION ( 'NONE',  ( -0.000000000000000000, -0.000000000000000000, -1.000000000000000000 ) ) ;
#12823 = CARTESIAN_POINT ( 'NONE',  ( -102.5926225674731569, 65.58224449241410525, -20.00000000000000355 ) ) ;
#12824 = ORIENTED_EDGE ( 'NONE', *, *, #8997, .T. ) ;
#12825 = EDGE_CURVE ( 'NONE', #4352, #3936, #11020, .T. ) ;
#12826 = DIRECTION ( 'NONE',  ( 0.000000000000000000, 0.000000000000000000, -1.000000000000000000 ) ) ;
#12827 = EDGE_CURVE ( 'NONE', #4520, #7041, #15991, .T. ) ;
#12828 = VERTEX_POINT ( 'NONE', #2502 ) ;
#12829 = EDGE_CURVE ( 'NONE', #10484, #9665, #8210, .T. ) ;
#12830 = DIRECTION ( 'NONE',  ( -0.9396926207859084279, 0.3420201433256686574, 1.086737899652989892E-16 ) ) ;
#12831 = MANIFOLD_SOLID_BREP ( 'Move Face6', #15367 ) ;
#12832 = CARTESIAN_POINT ( 'NONE',  ( -71.24615306438117557, 2.828944715229236628, -167.1454815528550739 ) ) ;
#12833 = ORIENTED_EDGE ( 'NONE', *, *, #16753, .T. ) ;
#12834 = VECTOR ( 'NONE', #10675, 1000.000000000000000 ) ;
#12835 = ORIENTED_EDGE ( 'NONE', *, *, #2665, .T. ) ;
#12836 = VERTEX_POINT ( 'NONE', #6713 ) ;
#12837 = UNCERTAINTY_MEASURE_WITH_UNIT (LENGTH_MEASURE( 1.000000000000000082E-05 ), #6501, 'distance_accuracy_value', 'NONE');
#12838 = EDGE_CURVE ( 'NONE', #4644, #15057, #16583, .T. ) ;
#12839 = ADVANCED_FACE ( 'NONE', ( #2692 ), #14015, .T. ) ;
#12840 = EDGE_CURVE ( 'NONE', #9223, #16505, #10882, .T. ) ;
#12841 = CARTESIAN_POINT ( 'NONE',  ( -71.24615306438076345, 126.2399288045637462, -167.1454815528550739 ) ) ;
#12842 = CARTESIAN_POINT ( 'NONE',  ( 7.349987227641307482E-14, -5.469921996229923700, 3.525817189091461579 ) ) ;
#12843 = LINE ( 'NONE', #9936, #9540 ) ;
#12844 = ADVANCED_FACE ( 'NONE', ( #17391 ), #9253, .T. ) ;
#12845 = LINE ( 'NONE', #10, #1501 ) ;
#12846 = CARTESIAN_POINT ( 'NONE',  ( -31.03642545851250745, 84.22855780814606419, 37.50000000000000000 ) ) ;
#12847 = VERTEX_POINT ( 'NONE', #9172 ) ;
#12848 = AXIS2_PLACEMENT_3D ( 'NONE', #15818, #5972, #3095 ) ;
#12849 = DIRECTION ( 'NONE',  ( 1.156482317317869999E-16, 0.000000000000000000, 1.000000000000000000 ) ) ;
#12850 = ORIENTED_EDGE ( 'NONE', *, *, #15594, .F. ) ;
#12851 = CARTESIAN_POINT ( 'NONE',  ( -59.05157857372951469, 96.57209730311865314, 15.00000000000006928 ) ) ;
#12852 = AXIS2_PLACEMENT_3D ( 'NONE', #2969, #10259, #14646 ) ;
#12853 = CARTESIAN_POINT ( 'NONE',  ( 4.699999999999995737, 3.752776749732559924, -6.500000000000061284 ) ) ;
#12854 = ORIENTED_EDGE ( 'NONE', *, *, #4863, .F. ) ;
#12855 = CARTESIAN_POINT ( 'NONE',  ( -113.8539578924277293, -92.35432678654407823, -7.309977258218748553 ) ) ;
#12856 = EDGE_CURVE ( 'NONE', #3722, #8797, #14858, .T. ) ;
#12857 = ORIENTED_EDGE ( 'NONE', *, *, #1507, .T. ) ;
#12858 = EDGE_CURVE ( 'NONE', #2137, #16012, #3539, .T. ) ;
#12859 = VECTOR ( 'NONE', #8268, 1000.000000000000000 ) ;
#12860 = EDGE_LOOP ( 'NONE', ( #17500, #4977, #3913, #12637, #7242, #8861 ) ) ;
#12861 = CIRCLE ( 'NONE', #8669, 4.599999999999999645 ) ;
#12862 = DIRECTION ( 'NONE',  ( 1.000000000000000000, -0.000000000000000000, -0.000000000000000000 ) ) ;
#12863 = CARTESIAN_POINT ( 'NONE',  ( -68.99615306438076345, 102.5409764881302408, 15.00000000000006928 ) ) ;
#12864 = DIRECTION ( 'NONE',  ( 0.000000000000000000, 5.551115123125748189E-17, 1.000000000000000000 ) ) ;
#12865 = ORIENTED_EDGE ( 'NONE', *, *, #12371, .F. ) ;
#12866 = ORIENTED_EDGE ( 'NONE', *, *, #2650, .F. ) ;
#12867 = CARTESIAN_POINT ( 'NONE',  ( -81.37409655828275845, -96.08423613455721579, 28.18308811886534571 ) ) ;
#12868 = ORIENTED_EDGE ( 'NONE', *, *, #15449, .T. ) ;
#12869 = LINE ( 'NONE', #8647, #10478 ) ;
#12870 = DIRECTION ( 'NONE',  ( 1.000000000000000000, 0.000000000000000000, 0.000000000000000000 ) ) ;
#12871 = CARTESIAN_POINT ( 'NONE',  ( -92.59262256747321373, 117.8748711238780373, -35.00000000000000000 ) ) ;
#12872 = ORIENTED_EDGE ( 'NONE', *, *, #8272, .F. ) ;
#12873 = AXIS2_PLACEMENT_3D ( 'NONE', #17228, #5720, #11544 ) ;
#12874 = DIRECTION ( 'NONE',  ( 7.442644330182800165E-16, -1.000000000000000000, 0.000000000000000000 ) ) ;
#12875 = ORIENTED_EDGE ( 'NONE', *, *, #6841, .F. ) ;
#12876 = AXIS2_PLACEMENT_3D ( 'NONE', #10299, #3185, #10382 ) ;
#12877 = ORIENTED_EDGE ( 'NONE', *, *, #10100, .F. ) ;
#12878 = VECTOR ( 'NONE', #15809, 1000.000000000000000 ) ;
#12879 = DIRECTION ( 'NONE',  ( -1.040834085586083310E-14, 0.000000000000000000, 1.000000000000000000 ) ) ;
#12880 = VERTEX_POINT ( 'NONE', #14590 ) ;
#12881 = ORIENTED_EDGE ( 'NONE', *, *, #17516, .F. ) ;
#12882 = VECTOR ( 'NONE', #11408, 1000.000000000000000 ) ;
#12883 = EDGE_LOOP ( 'NONE', ( #4494, #14386, #7101, #18239 ) ) ;
#12884 = AXIS2_PLACEMENT_3D ( 'NONE', #12654, #269, #1857 ) ;
#12885 = DIRECTION ( 'NONE',  ( 0.000000000000000000, 1.000000000000000000, 0.000000000000000000 ) ) ;
#12886 = ORIENTED_EDGE ( 'NONE', *, *, #3648, .T. ) ;
#12887 = CIRCLE ( 'NONE', #10767, 6.500000000000039968 ) ;
#12888 = DIRECTION ( 'NONE',  ( 1.000000000000000000, 0.000000000000000000, 5.551115123125786646E-16 ) ) ;
#12889 = CARTESIAN_POINT ( 'NONE',  ( -53.84898691462515785, 93.95493478196527803, -15.00000000000001421 ) ) ;
#12890 = VECTOR ( 'NONE', #7012, 1000.000000000000000 ) ;
#12891 = CARTESIAN_POINT ( 'NONE',  ( -57.08002265617300708, 84.22855780814606419, -61.50000000000001421 ) ) ;
#12892 = DIRECTION ( 'NONE',  ( 0.000000000000000000, 0.000000000000000000, -1.000000000000000000 ) ) ;
#12893 = EDGE_LOOP ( 'NONE', ( #8076, #2074, #3268, #12662 ) ) ;
#12894 = EDGE_CURVE ( 'NONE', #13601, #18188, #14944, .T. ) ;
#12895 = PLANE ( 'NONE',  #13782 ) ;
#12896 = DIRECTION ( 'NONE',  ( 1.000000000000000000, 0.000000000000000000, 0.000000000000000000 ) ) ;
#12897 = DIRECTION ( 'NONE',  ( 1.000000000000000000, 0.000000000000000000, 5.077734830647302671E-16 ) ) ;
#12898 = ORIENTED_EDGE ( 'NONE', *, *, #4803, .F. ) ;
#12899 = EDGE_CURVE ( 'NONE', #4262, #9354, #11965, .T. ) ;
#12900 = AXIS2_PLACEMENT_3D ( 'NONE', #4609, #2079, #1989 ) ;
#12901 = DIRECTION ( 'NONE',  ( -5.204170427930409450E-16, 0.000000000000000000, 1.000000000000000000 ) ) ;
#12902 = DIRECTION ( 'NONE',  ( -0.000000000000000000, 0.000000000000000000, 1.000000000000000000 ) ) ;
#12903 = DIRECTION ( 'NONE',  ( 1.000000000000000000, 0.000000000000000000, 0.000000000000000000 ) ) ;
#12904 = CIRCLE ( 'NONE', #2424, 12.50000000000001776 ) ;
#12905 = CIRCLE ( 'NONE', #6921, 10.38004356723770627 ) ;
#12906 = DIRECTION ( 'NONE',  ( 0.000000000000000000, 0.000000000000000000, 1.000000000000000000 ) ) ;
#12907 = ORIENTED_EDGE ( 'NONE', *, *, #10291, .T. ) ;
#12908 = ORIENTED_EDGE ( 'NONE', *, *, #15098, .F. ) ;
#12909 = CARTESIAN_POINT ( 'NONE',  ( -92.59262256747319952, 57.88796029049330372, 26.35917033480641436 ) ) ;
#12910 = VECTOR ( 'NONE', #2561, 1000.000000000000000 ) ;
#12911 = ORIENTED_EDGE ( 'NONE', *, *, #13961, .T. ) ;
#12912 = CARTESIAN_POINT ( 'NONE',  ( -57.08002265617300708, 84.22855780814606419, -62.50000000000000000 ) ) ;
#12913 = LINE ( 'NONE', #6755, #14146 ) ;
#12914 = LINE ( 'NONE', #15519, #12070 ) ;
#12915 = ORIENTED_EDGE ( 'NONE', *, *, #13113, .T. ) ;
#12916 = CARTESIAN_POINT ( 'NONE',  ( -92.59262256747319952, 50.58224449241410525, 35.00000000000000000 ) ) ;
#12917 = VECTOR ( 'NONE', #268, 1000.000000000000000 ) ;
#12918 = AXIS2_PLACEMENT_3D ( 'NONE', #17856, #7853, #12167 ) ;
#12919 = DIRECTION ( 'NONE',  ( 0.000000000000000000, 0.000000000000000000, -1.000000000000000000 ) ) ;
#12920 =( NAMED_UNIT ( * ) SI_UNIT ( $, .STERADIAN. ) SOLID_ANGLE_UNIT ( ) );
#12921 = LINE ( 'NONE', #18443, #16787 ) ;
#12922 = ORIENTED_EDGE ( 'NONE', *, *, #7340, .T. ) ;
#12923 = CARTESIAN_POINT ( 'NONE',  ( -52.04298920050707977, 93.78931001713317528, 15.00000000000006928 ) ) ;
#12924 = DIRECTION ( 'NONE',  ( -1.000000000000000000, -0.000000000000000000, -0.000000000000000000 ) ) ;
#12925 = ORIENTED_EDGE ( 'NONE', *, *, #2665, .F. ) ;
#12926 = CIRCLE ( 'NONE', #4820, 4.599999999999999645 ) ;
#12927 = EDGE_CURVE ( 'NONE', #10943, #12790, #14774, .T. ) ;
#12928 = DIRECTION ( 'NONE',  ( 0.000000000000000000, 0.000000000000000000, 1.000000000000000000 ) ) ;
#12929 = DIRECTION ( 'NONE',  ( 0.000000000000000000, 1.000000000000000000, 0.000000000000000000 ) ) ;
#12930 = ORIENTED_EDGE ( 'NONE', *, *, #4913, .F. ) ;
#12931 = APPLICATION_CONTEXT ( 'automotive_design' ) ;
#12932 = VERTEX_POINT ( 'NONE', #3264 ) ;
#12933 = AXIS2_PLACEMENT_3D ( 'NONE', #10160, #8864, #1655 ) ;
#12934 = AXIS2_PLACEMENT_3D ( 'NONE', #17772, #5234, #2326 ) ;
#12935 = CARTESIAN_POINT ( 'NONE',  ( 4.699999999999995737, -3.752776749732712691, -6.500000000000033751 ) ) ;
#12936 = LINE ( 'NONE', #107, #17120 ) ;
#12937 = EDGE_CURVE ( 'NONE', #5348, #17556, #1772, .T. ) ;
#12938 = CARTESIAN_POINT ( 'NONE',  ( -48.74405704658271077, 91.10542963993684396, 15.00000000000006928 ) ) ;
#12939 = EDGE_CURVE ( 'NONE', #689, #2737, #15998, .T. ) ;
#12940 = AXIS2_PLACEMENT_3D ( 'NONE', #1087, #9675, #1166 ) ;
#12941 = CARTESIAN_POINT ( 'NONE',  ( -46.03642545851250389, 84.22855780814606419, -61.50000000000001421 ) ) ;
#12942 = PLANE ( 'NONE',  #15593 ) ;
#12943 = ORIENTED_EDGE ( 'NONE', *, *, #4458, .F. ) ;
#12944 = DIRECTION ( 'NONE',  ( 1.000000000000000000, 0.000000000000000000, 6.950654929607132427E-15 ) ) ;
#12945 = ORIENTED_EDGE ( 'NONE', *, *, #3549, .T. ) ;
#12946 = CARTESIAN_POINT ( 'NONE',  ( -76.78641432137915501, -94.06000857856479058, 44.58117269483245337 ) ) ;
#12947 = AXIS2_PLACEMENT_3D ( 'NONE', #12178, #13584, #17868 ) ;
#12948 = CIRCLE ( 'NONE', #11150, 4.599999999999992539 ) ;
#12949 = DIRECTION ( 'NONE',  ( 0.9396926207859171987, 0.3420201433256444545, 0.000000000000000000 ) ) ;
#12950 = VERTEX_POINT ( 'NONE', #13199 ) ;
#12951 = EDGE_CURVE ( 'NONE', #13256, #12444, #13038, .T. ) ;
#12952 = ADVANCED_FACE ( 'NONE', ( #7480 ), #12068, .T. ) ;
#12953 = EDGE_CURVE ( 'NONE', #5917, #10355, #6067, .T. ) ;
#12954 = CARTESIAN_POINT ( 'NONE',  ( 49.38736944425943420, -141.5628872026273086, -57.00000000000000000 ) ) ;
#12955 = AXIS2_PLACEMENT_3D ( 'NONE', #1062, #3758, #6658 ) ;
#12956 = ORIENTED_EDGE ( 'NONE', *, *, #8594, .F. ) ;
#12957 = ADVANCED_FACE ( 'NONE', ( #14678 ), #7579, .T. ) ;
#12958 = VECTOR ( 'NONE', #12665, 1000.000000000000000 ) ;
#12959 = VECTOR ( 'NONE', #15745, 1000.000000000000000 ) ;
#12960 = VECTOR ( 'NONE', #8122, 1000.000000000000000 ) ;
#12961 = LINE ( 'NONE', #13048, #2232 ) ;
#12962 = CARTESIAN_POINT ( 'NONE',  ( -42.53669312409158465, -91.08423613455721579, 5.654315315325685987 ) ) ;
#12963 = LINE ( 'NONE', #5992, #5450 ) ;
#12964 = EDGE_LOOP ( 'NONE', ( #6722, #3522, #10491, #12191 ) ) ;
#12965 = EDGE_CURVE ( 'NONE', #17050, #5068, #17769, .T. ) ;
#12966 = CARTESIAN_POINT ( 'NONE',  ( -25.97029152202262026, -94.42547236494613117, 5.919112892686011484 ) ) ;
#12967 = ADVANCED_FACE ( 'NONE', ( #549, #6239 ), #17566, .F. ) ;
#12968 = VERTEX_POINT ( 'NONE', #15589 ) ;
#12969 = AXIS2_PLACEMENT_3D ( 'NONE', #4179, #11490, #1465 ) ;
#12970 = DIRECTION ( 'NONE',  ( 0.000000000000000000, 0.000000000000000000, 1.000000000000000000 ) ) ;
#12971 = FACE_OUTER_BOUND ( 'NONE', #6275, .T. ) ;
#12972 = CARTESIAN_POINT ( 'NONE',  ( -92.59262256747321373, 107.8748711238780373, -35.00000000000000000 ) ) ;
#12973 = EDGE_LOOP ( 'NONE', ( #4714, #7158, #4512, #1447, #3507, #1216, #236 ) ) ;
#12974 = PLANE ( 'NONE',  #9856 ) ;
#12975 = ORIENTED_EDGE ( 'NONE', *, *, #11897, .F. ) ;
#12976 = EDGE_CURVE ( 'NONE', #17429, #11961, #2221, .T. ) ;
#12977 = VECTOR ( 'NONE', #2322, 1000.000000000000000 ) ;
#12979 = ORIENTED_EDGE ( 'NONE', *, *, #9394, .T. ) ;
#12978 = VECTOR ( 'NONE', #11936, 1000.000000000000000 ) ;
#12980 = ORIENTED_EDGE ( 'NONE', *, *, #15071, .F. ) ;
#12981 = DIRECTION ( 'NONE',  ( -0.000000000000000000, -0.000000000000000000, -1.000000000000000000 ) ) ;
#12982 = CARTESIAN_POINT ( 'NONE',  ( -71.24615306438079188, 91.68240965456378433, 15.00000000000006928 ) ) ;
#12983 = ORIENTED_EDGE ( 'NONE', *, *, #11114, .T. ) ;
#12984 = VECTOR ( 'NONE', #9056, 1000.000000000000000 ) ;
#12985 = LINE ( 'NONE', #10150, #12241 ) ;
#12987 = VECTOR ( 'NONE', #13585, 1000.000000000000114 ) ;
#12986 = DIRECTION ( 'NONE',  ( 0.000000000000000000, 0.000000000000000000, 1.000000000000000000 ) ) ;
#12988 = CARTESIAN_POINT ( 'NONE',  ( -71.24615306438069240, 119.9567435045637893, 15.00000000000006928 ) ) ;
#12989 = FACE_OUTER_BOUND ( 'NONE', #5331, .T. ) ;
#12990 = ORIENTED_EDGE ( 'NONE', *, *, #8129, .F. ) ;
#12991 = DIRECTION ( 'NONE',  ( -0.000000000000000000, -0.000000000000000000, -1.000000000000000000 ) ) ;
#12992 = CARTESIAN_POINT ( 'NONE',  ( -71.24615306438080609, 115.9262801152292042, 15.00000000000006928 ) ) ;
#12993 = DIRECTION ( 'NONE',  ( 4.124608743189000987E-16, -1.000000000000000000, 0.000000000000000000 ) ) ;
#12994 = EDGE_LOOP ( 'NONE', ( #8206, #3736, #943, #13140 ) ) ;
#12995 = CLOSED_SHELL ( 'NONE', ( #14404, #4130, #2893, #15117, #8034, #17785, #361, #11087, #3759, #15903, #2938, #4998, #14402, #4150, #5398, #7418, #14532, #5622, #14544, #14309, #1186, #13991, #5508, #9156, #13377, #5481, #12579, #10649, #6513, #12270, #16694, #3893, #918, #2400, #8603, #10194 ) ) ;
#12996 = DIRECTION ( 'NONE',  ( 1.000000000000000000, 0.000000000000000000, 3.771137991253923150E-16 ) ) ;
#12997 = AXIS2_PLACEMENT_3D ( 'NONE', #2676, #14002, #15685 ) ;
#12998 = CARTESIAN_POINT ( 'NONE',  ( -68.99615306438100504, 42.23586028166270978, 15.00000000000006928 ) ) ;
#12999 = VECTOR ( 'NONE', #581, 1000.000000000000114 ) ;
#13000 = VECTOR ( 'NONE', #4280, 1000.000000000000000 ) ;
#13001 = ORIENTED_EDGE ( 'NONE', *, *, #5739, .F. ) ;
#13002 = AXIS2_PLACEMENT_3D ( 'NONE', #3739, #15137, #7575 ) ;
#13003 = PRODUCT_RELATED_PRODUCT_CATEGORY ( 'part', '', ( #6207 ) ) ;
#13004 = EDGE_LOOP ( 'NONE', ( #9342, #16790, #13907, #5541 ) ) ;
#13005 = DIRECTION ( 'NONE',  ( 0.000000000000000000, 1.000000000000000000, 0.000000000000000000 ) ) ;
#13006 = CIRCLE ( 'NONE', #15058, 172.7605492041889477 ) ;
#13007 = CARTESIAN_POINT ( 'NONE',  ( -64.09025127992788384, 50.58224449241410525, 28.00000000000000355 ) ) ;
#13008 = CARTESIAN_POINT ( 'NONE',  ( -64.09091675475967520, -93.09900487505510114, -43.93281256380662114 ) ) ;
#13009 = EDGE_LOOP ( 'NONE', ( #4997, #4115, #4875, #7495 ) ) ;
#13010 = AXIS2_PLACEMENT_3D ( 'NONE', #11930, #17903, #887 ) ;
#13011 = CARTESIAN_POINT ( 'NONE',  ( -57.08002265617300708, 84.22855780814606419, 77.50000000000000000 ) ) ;
#13012 = CARTESIAN_POINT ( 'NONE',  ( -57.08002265617300708, 84.22855780814606419, 15.00000000000006928 ) ) ;
#13013 = CARTESIAN_POINT ( 'NONE',  ( -92.59262256747321373, 117.8748711238780373, 35.00000000000000000 ) ) ;
#13014 = CIRCLE ( 'NONE', #4917, 29.36884788726140627 ) ;
#13015 = CARTESIAN_POINT ( 'NONE',  ( -71.24615306438070661, 135.6647067545637242, -167.1454815528550739 ) ) ;
#13016 = ORIENTED_EDGE ( 'NONE', *, *, #3781, .F. ) ;
#13017 = CARTESIAN_POINT ( 'NONE',  ( -57.08002265617300708, 84.22855780814606419, -15.00000000000001421 ) ) ;
#13018 = DIRECTION ( 'NONE',  ( 0.000000000000000000, 0.000000000000000000, 1.000000000000000000 ) ) ;
#13019 = ORIENTED_EDGE ( 'NONE', *, *, #5948, .F. ) ;
#13020 = CARTESIAN_POINT ( 'NONE',  ( -53.53072411395612562, 94.43552448259771381, 15.00000000000006928 ) ) ;
#13021 = CARTESIAN_POINT ( 'NONE',  ( -68.99615306438070661, 136.4836397816626743, 15.00000000000006928 ) ) ;
#13022 = VERTEX_POINT ( 'NONE', #14279 ) ;
#13023 = ORIENTED_EDGE ( 'NONE', *, *, #5293, .F. ) ;
#13024 = AXIS2_PLACEMENT_3D ( 'NONE', #16083, #7402, #562 ) ;
#13025 = AXIS2_PLACEMENT_3D ( 'NONE', #3170, #8881, #451 ) ;
#13026 = AXIS2_PLACEMENT_3D ( 'NONE', #14832, #7823, #12043 ) ;
#13027 = ORIENTED_EDGE ( 'NONE', *, *, #16947, .F. ) ;
#13028 = CARTESIAN_POINT ( 'NONE',  ( -65.06546592763139358, -96.08423613455721579, 28.18308811886540610 ) ) ;
#13029 = CARTESIAN_POINT ( 'NONE',  ( -68.99615306438090556, 74.26664263813029265, -15.00000000000001421 ) ) ;
#13030 = CARTESIAN_POINT ( 'NONE',  ( -68.99615306438072082, 130.8153103381302742, -167.1454815528550739 ) ) ;
#13031 = EDGE_CURVE ( 'NONE', #13368, #17232, #6694, .T. ) ;
#13032 = DIRECTION ( 'NONE',  ( 0.000000000000000000, 1.000000000000000000, 0.000000000000000000 ) ) ;
#13033 = LINE ( 'NONE', #4492, #6613 ) ;
#13034 = ORIENTED_EDGE ( 'NONE', *, *, #6220, .F. ) ;
#13035 = CARTESIAN_POINT ( 'NONE',  ( -57.08002265617300708, 84.22855780814606419, -15.00000000000001421 ) ) ;
#13036 = ORIENTED_EDGE ( 'NONE', *, *, #9273, .F. ) ;
#13037 = CARTESIAN_POINT ( 'NONE',  ( -81.11364370225147979, -91.08930958056578220, 39.31393734470474755 ) ) ;
#13038 = CIRCLE ( 'NONE', #10290, 4.600000000000006750 ) ;
#13039 = AXIS2_PLACEMENT_3D ( 'NONE', #15026, #16420, #17920 ) ;
#13040 = LINE ( 'NONE', #5548, #13751 ) ;
#13041 = VERTEX_POINT ( 'NONE', #14191 ) ;
#13042 = DIRECTION ( 'NONE',  ( 0.000000000000000000, 0.000000000000000000, -1.000000000000000000 ) ) ;
#13043 = CARTESIAN_POINT ( 'NONE',  ( -115.7702289486887395, -96.08423613455721579, -5.654315315326000402 ) ) ;
#13044 = VERTEX_POINT ( 'NONE', #12510 ) ;
#13045 = EDGE_CURVE ( 'NONE', #6896, #1716, #14094, .T. ) ;
#13046 = EDGE_CURVE ( 'NONE', #6830, #7572, #7026, .T. ) ;
#13047 = ORIENTED_EDGE ( 'NONE', *, *, #5010, .T. ) ;
#13048 = CARTESIAN_POINT ( 'NONE',  ( -123.4618227840623632, -111.0842361345572158, -57.00000000000000000 ) ) ;
#13049 = LINE ( 'NONE', #14264, #9688 ) ;
#13050 = DIRECTION ( 'NONE',  ( 0.000000000000000000, 1.000000000000000000, 0.000000000000000000 ) ) ;
#13051 = EDGE_CURVE ( 'NONE', #10924, #5018, #15294, .T. ) ;
#13052 = ORIENTED_EDGE ( 'NONE', *, *, #1227, .T. ) ;
#13053 = ADVANCED_FACE ( 'NONE', ( #5290 ), #13882, .F. ) ;
#13054 = ORIENTED_EDGE ( 'NONE', *, *, #4109, .F. ) ;
#13055 = SHAPE_REPRESENTATION ( 'Lower Replaceable Die Bushing', ( #16217 ), #17131 ) ;
#13056 = DIRECTION ( 'NONE',  ( -1.000000000000000000, 0.000000000000000000, 0.000000000000000000 ) ) ;
#13057 = DIRECTION ( 'NONE',  ( 0.000000000000000000, 0.000000000000000000, 1.000000000000000000 ) ) ;
#13058 = CARTESIAN_POINT ( 'NONE',  ( -198.5768363665157494, 84.22855780814606419, 62.50000000000001421 ) ) ;
#13059 = CARTESIAN_POINT ( 'NONE',  ( -61.98305514952129158, 93.22868410554717400, -15.00000000000001421 ) ) ;
#13060 = ORIENTED_EDGE ( 'NONE', *, *, #1705, .F. ) ;
#13061 = CARTESIAN_POINT ( 'NONE',  ( -57.99147934508202695, 74.02016676429184372, 15.00000000000006928 ) ) ;
#13062 = ORIENTED_EDGE ( 'NONE', *, *, #11909, .T. ) ;
#13063 = EDGE_CURVE ( 'NONE', #10938, #13044, #2774, .T. ) ;
#13064 = ORIENTED_EDGE ( 'NONE', *, *, #3420, .T. ) ;
#13065 = EDGE_CURVE ( 'NONE', #6083, #9555, #1377, .T. ) ;
#13066 = EDGE_CURVE ( 'NONE', #15720, #2855, #17078, .T. ) ;
#13067 = EDGE_CURVE ( 'NONE', #12093, #7210, #8574, .T. ) ;
#13068 = ORIENTED_EDGE ( 'NONE', *, *, #9186, .T. ) ;
#13069 = CARTESIAN_POINT ( 'NONE',  ( -68.99615306438117557, 4.536748481662661092, -167.1454815528550739 ) ) ;
#13070 = DIRECTION ( 'NONE',  ( 1.000000000000000000, 0.000000000000000000, 0.000000000000000000 ) ) ;
#13071 = EDGE_CURVE ( 'NONE', #12065, #6928, #18205, .T. ) ;
#13072 = ORIENTED_EDGE ( 'NONE', *, *, #13267, .F. ) ;
#13073 = EDGE_CURVE ( 'NONE', #6976, #16629, #16914, .T. ) ;
#13074 = DIRECTION ( 'NONE',  ( 0.9396926207859185309, 0.3420201433256406798, 4.890320548438501168E-16 ) ) ;
#13075 = CARTESIAN_POINT ( 'NONE',  ( -71.24615306438114715, 9.112130015229229940, -167.1454815528550739 ) ) ;
#13076 = CARTESIAN_POINT ( 'NONE',  ( -61.98611128973170992, 74.59995546124152099, 15.00000000000006928 ) ) ;
#13077 = CARTESIAN_POINT ( 'NONE',  ( -71.24615306438096241, 47.70011255456377341, 15.00000000000006928 ) ) ;
#13078 = ORIENTED_EDGE ( 'NONE', *, *, #14855, .T. ) ;
#13079 = LINE ( 'NONE', #8668, #18257 ) ;
#13080 = DIRECTION ( 'NONE',  ( 0.000000000000000000, 1.734723475976811433E-15, 1.000000000000000000 ) ) ;
#13081 = ORIENTED_EDGE ( 'NONE', *, *, #17719, .T. ) ;
#13082 = DIRECTION ( 'NONE',  ( 0.000000000000000000, 0.000000000000000000, 1.000000000000000000 ) ) ;
#13083 = DIRECTION ( 'NONE',  ( -1.000000000000000000, 0.000000000000000000, 0.000000000000000000 ) ) ;
#13084 = ORIENTED_EDGE ( 'NONE', *, *, #14579, .F. ) ;
#13085 = EDGE_CURVE ( 'NONE', #9307, #4088, #12605, .T. ) ;
#13086 = EDGE_CURVE ( 'NONE', #11956, #14266, #5371, .T. ) ;
#13087 = ORIENTED_EDGE ( 'NONE', *, *, #6599, .T. ) ;
#13088 = DIRECTION ( 'NONE',  ( 0.000000000000000000, 0.000000000000000000, -1.000000000000000000 ) ) ;
#13089 = CARTESIAN_POINT ( 'NONE',  ( 0.000000000000000000, 0.000000000000000000, 0.000000000000000000 ) ) ;
#13090 = LINE ( 'NONE', #5951, #5169 ) ;
#13091 = DIRECTION ( 'NONE',  ( 0.000000000000000000, 0.000000000000000000, -1.000000000000000000 ) ) ;
#13092 = EDGE_LOOP ( 'NONE', ( #14031, #698, #694, #5796 ) ) ;
#13093 = CARTESIAN_POINT ( 'NONE',  ( -71.24615306438070661, 147.3422066152292871, 15.00000000000006928 ) ) ;
#13094 = CARTESIAN_POINT ( 'NONE',  ( -69.66239992860627694, 84.22855780814606419, 25.00000000000000355 ) ) ;
#13095 = FACE_OUTER_BOUND ( 'NONE', #10705, .T. ) ;
#13096 = CARTESIAN_POINT ( 'NONE',  ( -208.2552686774341737, 84.22855780814606419, 69.87263542926429238 ) ) ;
#13097 = CARTESIAN_POINT ( 'NONE',  ( -37.32251732790476950, 91.47285552305426393, 60.54271558974930656 ) ) ;
#13098 = CARTESIAN_POINT ( 'NONE',  ( -66.88945454405379110, 81.25920652595873150, 15.00000000000006928 ) ) ;
#13099 = ORIENTED_EDGE ( 'NONE', *, *, #16449, .F. ) ;
#13100 = DIRECTION ( 'NONE',  ( 1.000000000000000000, 0.000000000000000000, 3.771137991253934490E-16 ) ) ;
#13101 = LINE ( 'NONE', #14322, #15796 ) ;
#13102 = EDGE_LOOP ( 'NONE', ( #8057, #10735, #4017, #17901 ) ) ;
#13103 = ORIENTED_EDGE ( 'NONE', *, *, #8486, .T. ) ;
#13104 = VECTOR ( 'NONE', #13688, 1000.000000000000000 ) ;
#13105 = ORIENTED_EDGE ( 'NONE', *, *, #5121, .F. ) ;
#13106 = DIRECTION ( 'NONE',  ( 1.156482317317869999E-16, 0.000000000000000000, 1.000000000000000000 ) ) ;
#13107 = LINE ( 'NONE', #13029, #13235 ) ;
#13108 = DIRECTION ( 'NONE',  ( 0.9396926207859097602, 0.3420201433256649381, 4.890320548438455808E-16 ) ) ;
#13109 = DIRECTION ( 'NONE',  ( 0.000000000000000000, 0.000000000000000000, 1.000000000000000000 ) ) ;
#13110 = LINE ( 'NONE', #550, #13154 ) ;
#13111 = CARTESIAN_POINT ( 'NONE',  ( 5.299999999999998934, 3.752776749732435135, 6.499999999999981348 ) ) ;
#13112 = EDGE_LOOP ( 'NONE', ( #3807, #5815, #1811, #16492, #4805, #7534 ) ) ;
#13113 = EDGE_CURVE ( 'NONE', #12209, #12621, #13910, .T. ) ;
#13114 = CARTESIAN_POINT ( 'NONE',  ( -68.99615306438094819, 71.12504998813029999, 15.00000000000006928 ) ) ;
#13115 = LINE ( 'NONE', #10850, #6978 ) ;
#13116 = PLANE ( 'NONE',  #5069 ) ;
#13117 = VECTOR ( 'NONE', #10759, 1000.000000000000000 ) ;
#13118 = ORIENTED_EDGE ( 'NONE', *, *, #5496, .F. ) ;
#13119 = DIRECTION ( 'NONE',  ( 1.156482317317869999E-16, 0.000000000000000000, 1.000000000000000000 ) ) ;
#13120 = DIRECTION ( 'NONE',  ( -0.000000000000000000, -0.000000000000000000, -1.000000000000000000 ) ) ;
#13121 = ORIENTED_EDGE ( 'NONE', *, *, #6169, .F. ) ;
#13122 = ORIENTED_EDGE ( 'NONE', *, *, #8841, .F. ) ;
#13123 = DIRECTION ( 'NONE',  ( -1.000000000000000000, 0.000000000000000000, 0.000000000000000000 ) ) ;
#13124 = AXIS2_PLACEMENT_3D ( 'NONE', #7432, #7526, #11837 ) ;
#13125 = CARTESIAN_POINT ( 'NONE',  ( -71.24615306438094819, 68.80239036522922902, 15.00000000000006928 ) ) ;
#13126 = CARTESIAN_POINT ( 'NONE',  ( -68.99615306438097662, 61.70027203813028649, -167.1454815528550739 ) ) ;
#13127 = ORIENTED_EDGE ( 'NONE', *, *, #8889, .T. ) ;
#13128 = EDGE_LOOP ( 'NONE', ( #8514, #11514, #458, #13551 ) ) ;
#13129 = CARTESIAN_POINT ( 'NONE',  ( -50.06979403241810900, 50.58224449241409104, 26.91246033477412425 ) ) ;
#13130 = CARTESIAN_POINT ( 'NONE',  ( -71.24615306438097662, 59.37761241522920841, 15.00000000000006928 ) ) ;
#13131 = DIRECTION ( 'NONE',  ( 0.000000000000000000, -0.000000000000000000, -1.000000000000000000 ) ) ;
#13132 = CARTESIAN_POINT ( 'NONE',  ( -52.17393402261416213, 74.59995546124159205, -15.00000000000001421 ) ) ;
#13133 = ORIENTED_EDGE ( 'NONE', *, *, #16152, .T. ) ;
#13134 = CARTESIAN_POINT ( 'NONE',  ( -68.99615306438100504, 42.23586028166270978, -15.00000000000001421 ) ) ;
#13135 = ORIENTED_EDGE ( 'NONE', *, *, #2974, .F. ) ;
#13136 = ORIENTED_EDGE ( 'NONE', *, *, #14096, .F. ) ;
#13137 = VECTOR ( 'NONE', #10336, 1000.000000000000000 ) ;
#13138 = EDGE_CURVE ( 'NONE', #7404, #7872, #5517, .T. ) ;
#13139 = VECTOR ( 'NONE', #3046, 1000.000000000000000 ) ;
#13140 = ORIENTED_EDGE ( 'NONE', *, *, #5617, .F. ) ;
#13141 = CARTESIAN_POINT ( 'NONE',  ( -57.08002265617300708, 84.22855780814606419, 37.50000000000000000 ) ) ;
#13142 = DIRECTION ( 'NONE',  ( 0.000000000000000000, 0.000000000000000000, 1.000000000000000000 ) ) ;
#13143 = VERTEX_POINT ( 'NONE', #8656 ) ;
#13144 = EDGE_CURVE ( 'NONE', #3936, #4543, #4355, .T. ) ;
#13145 = DIRECTION ( 'NONE',  ( 1.000000000000000000, 0.000000000000000000, 0.000000000000000000 ) ) ;
#13146 = CARTESIAN_POINT ( 'NONE',  ( 276.3098885457529832, -32.62665103886256190, -7.000000000000010658 ) ) ;
#13147 = CARTESIAN_POINT ( 'NONE',  ( -57.74389692835771370, 95.01461175692088545, -167.1454815528550739 ) ) ;
#13149 = EDGE_CURVE ( 'NONE', #15640, #7354, #15766, .T. ) ;
#13148 = AXIS2_PLACEMENT_3D ( 'NONE', #14952, #17574, #17671 ) ;
#13150 = DIRECTION ( 'NONE',  ( -3.223492141267075737E-15, 0.000000000000000000, 1.000000000000000000 ) ) ;
#13151 = ORIENTED_EDGE ( 'NONE', *, *, #5133, .F. ) ;
#13152 = ADVANCED_FACE ( 'NONE', ( #5752 ), #4022, .F. ) ;
#13153 = FACE_OUTER_BOUND ( 'NONE', #14071, .T. ) ;
#13154 = VECTOR ( 'NONE', #5974, 1000.000000000000000 ) ;
#13155 = CARTESIAN_POINT ( 'NONE',  ( -57.08002265617300708, 84.22855780814606419, 92.50000000000000000 ) ) ;
#13156 = DIRECTION ( 'NONE',  ( 0.000000000000000000, 0.000000000000000000, 1.000000000000000000 ) ) ;
#13157 = ORIENTED_EDGE ( 'NONE', *, *, #12965, .F. ) ;
#13158 = LINE ( 'NONE', #15783, #10600 ) ;
#13159 = EDGE_CURVE ( 'NONE', #11181, #1460, #8015, .T. ) ;
#13160 = VECTOR ( 'NONE', #4192, 1000.000000000000000 ) ;
#13161 = EDGE_CURVE ( 'NONE', #4254, #17707, #12054, .T. ) ;
#13162 = PLANE ( 'NONE',  #11352 ) ;
#13163 = EDGE_CURVE ( 'NONE', #9789, #2703, #15128, .T. ) ;
#13164 = EDGE_LOOP ( 'NONE', ( #12898, #4096 ) ) ;
#13165 = AXIS2_PLACEMENT_3D ( 'NONE', #7654, #14666, #16061 ) ;
#13166 = ORIENTED_EDGE ( 'NONE', *, *, #3652, .T. ) ;
#13167 = EDGE_CURVE ( 'NONE', #13281, #3722, #15218, .T. ) ;
#13168 = CIRCLE ( 'NONE', #13765, 45.40389983439752086 ) ;
#13169 = TOROIDAL_SURFACE ( 'NONE', #10768, 7.372635429264279061, 4.962965561209096599 ) ;
#13170 = VERTEX_POINT ( 'NONE', #9157 ) ;
#13171 = DIRECTION ( 'NONE',  ( 0.000000000000000000, 0.000000000000000000, 1.000000000000000000 ) ) ;
#13172 = EDGE_CURVE ( 'NONE', #16713, #13980, #7937, .T. ) ;
#13173 = ORIENTED_EDGE ( 'NONE', *, *, #7003, .F. ) ;
#13174 = DIRECTION ( 'NONE',  ( 1.000000000000000000, 0.000000000000000000, 0.000000000000000000 ) ) ;
#13175 = CARTESIAN_POINT ( 'NONE',  ( -66.17173038963701970, 112.1547175742259697, -26.82650548119792688 ) ) ;
#13176 = CARTESIAN_POINT ( 'NONE',  ( -67.59262256747315689, 111.6514400295689313, 37.50000000000000000 ) ) ;
#13177 = VERTEX_POINT ( 'NONE', #2404 ) ;
#13178 = CARTESIAN_POINT ( 'NONE',  ( -71.24615306438090556, 60.26648315456375826, 15.00000000000006928 ) ) ;
#13179 = LINE ( 'NONE', #16332, #7934 ) ;
#13180 = EDGE_CURVE ( 'NONE', #15619, #14794, #14843, .T. ) ;
#13181 = DIRECTION ( 'NONE',  ( 0.000000000000000000, 0.000000000000000000, 1.000000000000000000 ) ) ;
#13182 = DIRECTION ( 'NONE',  ( 0.000000000000000000, 0.000000000000000000, 1.000000000000000000 ) ) ;
#13183 = EDGE_CURVE ( 'NONE', #115, #13022, #2128, .T. ) ;
#13184 = CARTESIAN_POINT ( 'NONE',  ( -36.29766045040744160, 87.56553636334628266, 69.23463151675950655 ) ) ;
#13185 = AXIS2_PLACEMENT_3D ( 'NONE', #2003, #8073, #16493 ) ;
#13186 = CARTESIAN_POINT ( 'NONE',  ( -69.56651066787533466, 84.80960611389535586, -167.1454815528550739 ) ) ;
#13187 = ORIENTED_EDGE ( 'NONE', *, *, #5822, .T. ) ;
#13188 = CARTESIAN_POINT ( 'NONE',  ( -67.59262256747317110, 61.64996188551982215, 25.00000000000000355 ) ) ;
#13189 = CARTESIAN_POINT ( 'NONE',  ( -76.37409655828219002, -91.08423613455721579, -45.05044770573186952 ) ) ;
#13190 = VERTEX_POINT ( 'NONE', #8111 ) ;
#13191 = ORIENTED_EDGE ( 'NONE', *, *, #7918, .T. ) ;
#13192 = VECTOR ( 'NONE', #12944, 1000.000000000000000 ) ;
#13193 = ORIENTED_EDGE ( 'NONE', *, *, #2311, .T. ) ;
#13194 = VECTOR ( 'NONE', #13876, 1000.000000000000000 ) ;
#13195 = AXIS2_PLACEMENT_3D ( 'NONE', #14797, #12095, #3565 ) ;
#13196 = DIRECTION ( 'NONE',  ( -5.204170427930409450E-16, 0.000000000000000000, 1.000000000000000000 ) ) ;
#13197 = CARTESIAN_POINT ( 'NONE',  ( -107.5926225674731995, 60.58224449241411946, -35.00000000000000000 ) ) ;
#13198 = CARTESIAN_POINT ( 'NONE',  ( -78.11929946934434099, 83.73612801793909455, 55.01209612034283936 ) ) ;
#13199 = CARTESIAN_POINT ( 'NONE',  ( -71.24615306438109030, 27.96168591522921076, -15.00000000000001421 ) ) ;
#13200 = CYLINDRICAL_SURFACE ( 'NONE', #14636, 5.000000000000004441 ) ;
#13201 = DIRECTION ( 'NONE',  ( 4.029365176583844474E-15, -0.000000000000000000, -1.000000000000000000 ) ) ;
#13202 = CARTESIAN_POINT ( 'NONE',  ( -64.09025127992791226, 117.8748711238780373, 28.00000000000000355 ) ) ;
#13203 = ORIENTED_EDGE ( 'NONE', *, *, #6885, .F. ) ;
#13204 = FACE_OUTER_BOUND ( 'NONE', #11280, .T. ) ;
#13205 = CIRCLE ( 'NONE', #4808, 11.04359719766050141 ) ;
#13206 = CARTESIAN_POINT ( 'NONE',  ( -71.24615306438091977, 72.83285375456371469, -167.1454815528550739 ) ) ;
#13207 = LINE ( 'NONE', #17775, #14912 ) ;
#13208 = ORIENTED_EDGE ( 'NONE', *, *, #12346, .T. ) ;
#13209 = AXIS2_PLACEMENT_3D ( 'NONE', #5936, #15959, #3153 ) ;
#13210 = CARTESIAN_POINT ( 'NONE',  ( -68.99615306438106188, 36.56753083813027416, 15.00000000000006928 ) ) ;
#13211 = VECTOR ( 'NONE', #13872, 1000.000000000000000 ) ;
#13212 = CARTESIAN_POINT ( 'NONE',  ( -71.24615306438106188, 37.38646386522923137, 15.00000000000006928 ) ) ;
#13213 = ORIENTED_EDGE ( 'NONE', *, *, #12827, .F. ) ;
#13214 = EDGE_CURVE ( 'NONE', #12329, #8416, #13577, .T. ) ;
#13215 = ORIENTED_EDGE ( 'NONE', *, *, #6514, .F. ) ;
#13216 = AXIS2_PLACEMENT_3D ( 'NONE', #1825, #5084, #15003 ) ;
#13217 = CYLINDRICAL_SURFACE ( 'NONE', #7600, 10.24900000000000055 ) ;
#13218 = CARTESIAN_POINT ( 'NONE',  ( -45.07652969643970664, 51.92630754768256907, -25.99113068039098451 ) ) ;
#13219 = LINE ( 'NONE', #11462, #79 ) ;
#13220 = EDGE_LOOP ( 'NONE', ( #3746, #10440, #10811, #7273 ) ) ;
#13221 = EDGE_CURVE ( 'NONE', #18030, #12968, #536, .T. ) ;
#13222 = AXIS2_PLACEMENT_3D ( 'NONE', #9189, #6457, #14879 ) ;
#13223 = CIRCLE ( 'NONE', #7520, 4.962965561209093046 ) ;
#13224 = ORIENTED_EDGE ( 'NONE', *, *, #700, .T. ) ;
#13225 = DIRECTION ( 'NONE',  ( -0.000000000000000000, -1.000000000000000000, -0.000000000000000000 ) ) ;
#13226 = DIRECTION ( 'NONE',  ( 0.000000000000000000, 0.000000000000000000, 1.000000000000000000 ) ) ;
#13227 = FACE_OUTER_BOUND ( 'NONE', #618, .T. ) ;
#13228 = CARTESIAN_POINT ( 'NONE',  ( -44.89980253466632831, 81.41924511788819530, -15.00000000000001421 ) ) ;
#13229 = ORIENTED_EDGE ( 'NONE', *, *, #3450, .F. ) ;
#13230 = PLANE ( 'NONE',  #4457 ) ;
#13231 = ORIENTED_EDGE ( 'NONE', *, *, #2255, .T. ) ;
#13232 = AXIS2_PLACEMENT_3D ( 'NONE', #12115, #16390, #2187 ) ;
#13233 = DIRECTION ( 'NONE',  ( 0.3420201433256724322, 0.9396926207859070956, -0.000000000000000000 ) ) ;
#13234 = ORIENTED_EDGE ( 'NONE', *, *, #140, .T. ) ;
#13235 = VECTOR ( 'NONE', #15995, 1000.000000000000000 ) ;
#13236 = VECTOR ( 'NONE', #15675, 1000.000000000000000 ) ;
#13237 = EDGE_LOOP ( 'NONE', ( #4532, #11721, #8801, #1244, #9218, #14850, #2559, #13283, #6198, #10503, #2949, #13064, #12481, #15298, #2235, #14187, #13191 ) ) ;
#13238 = CARTESIAN_POINT ( 'NONE',  ( 15.23320273812466041, -19.34983604512934363, 54.79921157549236455 ) ) ;
#13239 = AXIS2_PLACEMENT_3D ( 'NONE', #4824, #4725, #17639 ) ;
#13240 = ORIENTED_EDGE ( 'NONE', *, *, #3189, .T. ) ;
#13241 = DIRECTION ( 'NONE',  ( 0.000000000000000000, 0.000000000000000000, 1.000000000000000000 ) ) ;
#13242 = DIRECTION ( 'NONE',  ( 1.000000000000000000, 0.000000000000000000, 0.000000000000000000 ) ) ;
#13243 = DIRECTION ( 'NONE',  ( 0.3420201433256686574, 0.9396926207859084279, -0.000000000000000000 ) ) ;
#13244 = ORIENTED_EDGE ( 'NONE', *, *, #6384, .F. ) ;
#13245 = EDGE_CURVE ( 'NONE', #7590, #14582, #5016, .T. ) ;
#13246 = CARTESIAN_POINT ( 'NONE',  ( -71.24615306438114715, 15.39531531522927921, -15.00000000000001421 ) ) ;
#13247 = AXIS2_PLACEMENT_3D ( 'NONE', #6345, #10753, #6247 ) ;
#13248 = CIRCLE ( 'NONE', #9656, 34.36884788726141693 ) ;
#13249 = LINE ( 'NONE', #3699, #6622 ) ;
#13250 = LINE ( 'NONE', #8671, #9330 ) ;
#13251 = ORIENTED_EDGE ( 'NONE', *, *, #18329, .F. ) ;
#13252 = CARTESIAN_POINT ( 'NONE',  ( -57.08002265617300708, 84.22855780814606419, -167.1454815528550739 ) ) ;
#13253 = FACE_BOUND ( 'NONE', #1080, .T. ) ;
#13254 = ORIENTED_EDGE ( 'NONE', *, *, #5675, .T. ) ;
#13255 = EDGE_CURVE ( 'NONE', #14173, #9962, #1665, .T. ) ;
#13256 = VERTEX_POINT ( 'NONE', #17650 ) ;
#13257 = AXIS2_PLACEMENT_3D ( 'NONE', #1103, #6796, #8294 ) ;
#13258 = VECTOR ( 'NONE', #5850, 1000.000000000000227 ) ;
#13259 = ORIENTED_EDGE ( 'NONE', *, *, #2911, .F. ) ;
#13260 = DIRECTION ( 'NONE',  ( -0.7930648017910726377, 0.6091372753001467188, 0.000000000000000000 ) ) ;
#13261 =( LENGTH_UNIT ( ) NAMED_UNIT ( * ) SI_UNIT ( .MILLI., .METRE. ) );
#13262 = DIRECTION ( 'NONE',  ( 0.000000000000000000, 0.000000000000000000, 1.000000000000000000 ) ) ;
#13263 = CARTESIAN_POINT ( 'NONE',  ( -68.99615306438100504, 45.99230878813026635, -167.1454815528550739 ) ) ;
#13264 = DIRECTION ( 'NONE',  ( -0.000000000000000000, -0.000000000000000000, 1.000000000000000000 ) ) ;
#13265 = FACE_OUTER_BOUND ( 'NONE', #15534, .T. ) ;
#13266 = ORIENTED_EDGE ( 'NONE', *, *, #1852, .F. ) ;
#13267 = EDGE_CURVE ( 'NONE', #14227, #11339, #738, .T. ) ;
#13268 = EDGE_CURVE ( 'NONE', #14752, #15269, #6090, .T. ) ;
#13269 = CARTESIAN_POINT ( 'NONE',  ( -71.24615306438080609, 116.8151508545637114, 15.00000000000006928 ) ) ;
#13270 = PLANE ( 'NONE',  #18406 ) ;
#13271 = DIRECTION ( 'NONE',  ( 0.9396926207859110924, 0.3420201433256612189, 4.890320548438462711E-16 ) ) ;
#13272 = FACE_OUTER_BOUND ( 'NONE', #8279, .T. ) ;
#13273 = CARTESIAN_POINT ( 'NONE',  ( -36.53760766897426038, 88.81248391902217065, 68.45606934554520251 ) ) ;
#13274 = AXIS2_PLACEMENT_3D ( 'NONE', #11212, #2960, #14011 ) ;
#13275 = VECTOR ( 'NONE', #17236, 1000.000000000000000 ) ;
#13276 = CARTESIAN_POINT ( 'NONE',  ( -76.06514409945376087, 73.26749283226919829, 92.50000000000000000 ) ) ;
#13277 = ORIENTED_EDGE ( 'NONE', *, *, #18213, .T. ) ;
#13278 = EDGE_CURVE ( 'NONE', #9072, #16289, #16337, .T. ) ;
#13279 = CARTESIAN_POINT ( 'NONE',  ( 15.23320273812466574, -111.0842361345572158, 57.00000000000000000 ) ) ;
#13280 = CARTESIAN_POINT ( 'NONE',  ( -36.20403484863803101, 81.56801578385648099, 55.48345971814259769 ) ) ;
#13281 = VERTEX_POINT ( 'NONE', #9434 ) ;
#13282 = EDGE_CURVE ( 'NONE', #11356, #14710, #5217, .T. ) ;
#13283 = ORIENTED_EDGE ( 'NONE', *, *, #4659, .T. ) ;
#13284 = AXIS2_PLACEMENT_3D ( 'NONE', #9860, #2749, #7499 ) ;
#13285 = EDGE_CURVE ( 'NONE', #7166, #2933, #17925, .T. ) ;
#13286 = EDGE_CURVE ( 'NONE', #7142, #4127, #17755, .T. ) ;
#13287 = VECTOR ( 'NONE', #15711, 1000.000000000000000 ) ;
#13288 = ORIENTED_EDGE ( 'NONE', *, *, #13113, .F. ) ;
#13289 = AXIS2_PLACEMENT_3D ( 'NONE', #6112, #11839, #4628 ) ;
#13290 = VECTOR ( 'NONE', #106, 1000.000000000000000 ) ;
#13291 = CARTESIAN_POINT ( 'NONE',  ( -44.59353464447068660, 84.80960611389554060, -15.00000000000001421 ) ) ;
#13292 = LINE ( 'NONE', #14588, #14150 ) ;
#13293 = CYLINDRICAL_SURFACE ( 'NONE', #17584, 4.600000000000006750 ) ;
#13294 = CARTESIAN_POINT ( 'NONE',  ( -71.24615306438091977, 75.97444640456376419, -167.1454815528550739 ) ) ;
#13295 = EDGE_CURVE ( 'NONE', #5082, #8042, #180, .T. ) ;
#13296 = CYLINDRICAL_SURFACE ( 'NONE', #17912, 4.000000000000024869 ) ;
#13297 = CARTESIAN_POINT ( 'NONE',  ( -71.24615306438086293, 100.2183168652291982, -167.1454815528550739 ) ) ;
#13298 = PLANE ( 'NONE',  #8731 ) ;
#13299 = ORIENTED_EDGE ( 'NONE', *, *, #3801, .F. ) ;
#13300 = CARTESIAN_POINT ( 'NONE',  ( -44.63071506687145984, 85.35316464920607871, -15.00000000000001421 ) ) ;
#13301 = DIRECTION ( 'NONE',  ( 1.000000000000000000, 0.000000000000000000, 0.000000000000000000 ) ) ;
#13302 = DIRECTION ( 'NONE',  ( 1.000000000000000000, 0.000000000000000000, 0.000000000000000000 ) ) ;
#13303 = ORIENTED_EDGE ( 'NONE', *, *, #11778, .T. ) ;
#13304 = AXIS2_PLACEMENT_3D ( 'NONE', #16177, #13383, #17674 ) ;
#13305 = PLANE ( 'NONE',  #13304 ) ;
#13306 = VECTOR ( 'NONE', #7852, 1000.000000000000114 ) ;
#13307 = LINE ( 'NONE', #765, #15192 ) ;
#13309 = ORIENTED_EDGE ( 'NONE', *, *, #14873, .T. ) ;
#13308 = AXIS2_PLACEMENT_3D ( 'NONE', #13635, #6417, #17827 ) ;
#13310 = ADVANCED_FACE ( 'NONE', ( #13646 ), #6515, .T. ) ;
#13311 = ORIENTED_EDGE ( 'NONE', *, *, #2651, .T. ) ;
#13312 = FACE_OUTER_BOUND ( 'NONE', #6823, .T. ) ;
#13313 = DIRECTION ( 'NONE',  ( 0.000000000000000000, 0.000000000000000000, 1.000000000000000000 ) ) ;
#13314 = DIRECTION ( 'NONE',  ( -1.000000000000000000, 0.000000000000000000, 0.000000000000000000 ) ) ;
#13315 = ORIENTED_EDGE ( 'NONE', *, *, #3214, .F. ) ;
#13316 = MECHANICAL_DESIGN_GEOMETRIC_PRESENTATION_REPRESENTATION (  '', ( #11822 ), #14505 ) ;
#13317 = VECTOR ( 'NONE', #10367, 1000.000000000000000 ) ;
#13318 = ORIENTED_EDGE ( 'NONE', *, *, #8100, .F. ) ;
#13319 = CARTESIAN_POINT ( 'NONE',  ( 15.23320273812467462, -111.0842361345572158, 3.000000000000000000 ) ) ;
#13320 = LINE ( 'NONE', #2168, #17080 ) ;
#13321 = PLANE ( 'NONE',  #15376 ) ;
#13322 = LINE ( 'NONE', #499, #15309 ) ;
#13323 = ORIENTED_EDGE ( 'NONE', *, *, #18306, .F. ) ;
#13324 = DIRECTION ( 'NONE',  ( -0.000000000000000000, 1.000000000000000000, -0.000000000000000000 ) ) ;
#13325 = ORIENTED_EDGE ( 'NONE', *, *, #14201, .F. ) ;
#13326 = CARTESIAN_POINT ( 'NONE',  ( -65.41598826576338865, 91.10542963993673027, -167.1454815528550739 ) ) ;
#13327 = VERTEX_POINT ( 'NONE', #16912 ) ;
#13328 = ORIENTED_EDGE ( 'NONE', *, *, #8250, .T. ) ;
#13329 = VERTEX_POINT ( 'NONE', #18505 ) ;
#13330 =( LENGTH_UNIT ( ) NAMED_UNIT ( * ) SI_UNIT ( .MILLI., .METRE. ) );
#13331 = CARTESIAN_POINT ( 'NONE',  ( -25.66933353722515676, -96.08423613455721579, 5.654315315325685987 ) ) ;
#13332 = VERTEX_POINT ( 'NONE', #14020 ) ;
#13333 = DIRECTION ( 'NONE',  ( 1.000000000000000000, 0.000000000000000000, 3.771137991253923150E-16 ) ) ;
#13334 = CARTESIAN_POINT ( 'NONE',  ( -42.53669312409158465, -96.08423613455721579, 10.65431531532568599 ) ) ;
#13335 = ORIENTED_EDGE ( 'NONE', *, *, #2430, .T. ) ;
#13336 = CARTESIAN_POINT ( 'NONE',  ( -71.24615306438080609, 106.5015021652292404, -167.1454815528550739 ) ) ;
#13337 = VERTEX_POINT ( 'NONE', #1015 ) ;
#13338 = PLANE ( 'NONE',  #5135 ) ;
#13339 = DIRECTION ( 'NONE',  ( 0.000000000000000000, 0.000000000000000000, 1.000000000000000000 ) ) ;
#13341 = ORIENTED_EDGE ( 'NONE', *, *, #11698, .T. ) ;
#13340 = EDGE_CURVE ( 'NONE', #2025, #9102, #12530, .T. ) ;
#13342 = CARTESIAN_POINT ( 'NONE',  ( -46.65463807863145007, 87.07303407725225952, -15.00000000000001421 ) ) ;
#13343 = LINE ( 'NONE', #7278, #4213 ) ;
#13344 = ORIENTED_EDGE ( 'NONE', *, *, #8358, .F. ) ;
#13345 = EDGE_LOOP ( 'NONE', ( #17587, #8022, #15843, #9724 ) ) ;
#13346 = ORIENTED_EDGE ( 'NONE', *, *, #6889, .T. ) ;
#13347 = LINE ( 'NONE', #16409, #12062 ) ;
#13348 = ORIENTED_EDGE ( 'NONE', *, *, #1053, .T. ) ;
#13349 = CARTESIAN_POINT ( 'NONE',  ( 0.000000000000000000, 0.000000000000000000, 0.000000000000000000 ) ) ;
#13350 = FACE_OUTER_BOUND ( 'NONE', #3881, .T. ) ;
#13351 = DIRECTION ( 'NONE',  ( 1.000000000000000000, 0.000000000000000000, 4.625929269271485914E-16 ) ) ;
#13352 = CARTESIAN_POINT ( 'NONE',  ( -71.24615306438080609, 107.3903729045637192, -167.1454815528550739 ) ) ;
#13353 = VERTEX_POINT ( 'NONE', #15611 ) ;
#13354 = CARTESIAN_POINT ( 'NONE',  ( -71.24615306438094819, 68.80239036522922902, -167.1454815528550739 ) ) ;
#13355 = CARTESIAN_POINT ( 'NONE',  ( -92.59262256747319952, 57.88796029049329661, -22.35917033480642502 ) ) ;
#13356 = CYLINDRICAL_SURFACE ( 'NONE', #8837, 7.500000000000000000 ) ;
#13357 = CARTESIAN_POINT ( 'NONE',  ( -68.99615306438077766, 124.5321250381302747, -167.1454815528550739 ) ) ;
#13358 = CARTESIAN_POINT ( 'NONE',  ( -36.03642545851251100, 84.47473112397162254, 70.00000000000002842 ) ) ;
#13359 = ORIENTED_EDGE ( 'NONE', *, *, #414, .F. ) ;
#13360 = DIRECTION ( 'NONE',  ( 1.000000000000000000, 0.000000000000000000, 0.000000000000000000 ) ) ;
#13361 = ORIENTED_EDGE ( 'NONE', *, *, #700, .F. ) ;
#13362 = CARTESIAN_POINT ( 'NONE',  ( -92.59262256747321373, 106.8071537307723133, 25.00000000000000000 ) ) ;
#13363 = LINE ( 'NONE', #17760, #1232 ) ;
#13364 = ORIENTED_EDGE ( 'NONE', *, *, #3164, .T. ) ;
#13365 = ORIENTED_EDGE ( 'NONE', *, *, #4452, .T. ) ;
#13366 = ADVANCED_FACE ( 'NONE', ( #11124 ), #9902, .T. ) ;
#13367 = EDGE_CURVE ( 'NONE', #11181, #9065, #12632, .T. ) ;
#13368 = VERTEX_POINT ( 'NONE', #15507 ) ;
#13369 = CARTESIAN_POINT ( 'NONE',  ( -57.08002265617300708, 84.22855780814606419, 28.00000000000000355 ) ) ;
#13370 = LINE ( 'NONE', #2239, #13834 ) ;
#13371 = DIRECTION ( 'NONE',  ( 0.3420201433256686574, -0.9396926207859084279, 0.000000000000000000 ) ) ;
#13372 = DIRECTION ( 'NONE',  ( 0.000000000000000000, 0.000000000000000000, -1.000000000000000000 ) ) ;
#13373 = EDGE_CURVE ( 'NONE', #17050, #9018, #11403, .T. ) ;
#13374 = DIRECTION ( 'NONE',  ( 0.000000000000000000, 1.000000000000000000, 0.000000000000000000 ) ) ;
#13375 = DIRECTION ( 'NONE',  ( 1.000000000000000000, 0.000000000000000000, 0.000000000000000000 ) ) ;
#13376 = VERTEX_POINT ( 'NONE', #6720 ) ;
#13377 = ADVANCED_FACE ( 'NONE', ( #18228 ), #13893, .T. ) ;
#13378 = EDGE_CURVE ( 'NONE', #794, #1345, #12806, .T. ) ;
#13379 = DIRECTION ( 'NONE',  ( 1.000000000000000000, 0.000000000000000000, 0.000000000000000000 ) ) ;
#13380 = CARTESIAN_POINT ( 'NONE',  ( -76.04777162888156283, 61.80621309083046100, -27.19272967165976596 ) ) ;
#13381 = PLANE ( 'NONE',  #4194 ) ;
#13382 = ORIENTED_EDGE ( 'NONE', *, *, #2067, .F. ) ;
#13383 = DIRECTION ( 'NONE',  ( -1.000000000000000000, 0.000000000000000000, 0.000000000000000000 ) ) ;
#13384 = CARTESIAN_POINT ( 'NONE',  ( -44.63071506687145984, 85.35316464920607871, -167.1454815528550739 ) ) ;
#13385 = ORIENTED_EDGE ( 'NONE', *, *, #17708, .T. ) ;
#13386 = AXIS2_PLACEMENT_3D ( 'NONE', #11715, #14522, #3110 ) ;
#13387 = EDGE_CURVE ( 'NONE', #7647, #15598, #16812, .T. ) ;
#13388 = ADVANCED_FACE ( 'NONE', ( #17000 ), #13826, .T. ) ;
#13389 = ADVANCED_FACE ( 'NONE', ( #17097 ), #11310, .T. ) ;
#13390 = ORIENTED_EDGE ( 'NONE', *, *, #820, .T. ) ;
#13391 = UNCERTAINTY_MEASURE_WITH_UNIT (LENGTH_MEASURE( 1.000000000000000082E-05 ), #9956, 'distance_accuracy_value', 'NONE');
#13392 = EDGE_CURVE ( 'NONE', #3197, #7512, #14216, .T. ) ;
#13393 = LINE ( 'NONE', #2338, #10305 ) ;
#13394 = DIRECTION ( 'NONE',  ( 0.000000000000000000, 0.000000000000000000, 1.000000000000000000 ) ) ;
#13395 = CARTESIAN_POINT ( 'NONE',  ( -68.99615306438086293, 92.50134268166266338, 15.00000000000006928 ) ) ;
#13396 = ORIENTED_EDGE ( 'NONE', *, *, #18208, .T. ) ;
#13397 = FACE_OUTER_BOUND ( 'NONE', #7384, .T. ) ;
#13398 = ORIENTED_EDGE ( 'NONE', *, *, #17888, .T. ) ;
#13399 = AXIS2_PLACEMENT_3D ( 'NONE', #1419, #7301, #4481 ) ;
#13400 = LINE ( 'NONE', #14611, #13778 ) ;
#13401 = DIRECTION ( 'NONE',  ( 0.000000000000000000, 0.000000000000000000, -1.000000000000000000 ) ) ;
#13402 = CARTESIAN_POINT ( 'NONE',  ( -50.35400969968294049, 73.69239390902568232, -15.00000000000001421 ) ) ;
#13403 = CARTESIAN_POINT ( 'NONE',  ( 7.405446926805384449E-14, -96.08423613455721579, -10.65431531532519571 ) ) ;
#13404 = VERTEX_POINT ( 'NONE', #12442 ) ;
#13405 = EDGE_CURVE ( 'NONE', #4483, #10712, #18134, .T. ) ;
#13406 = ADVANCED_FACE ( 'NONE', ( #11024 ), #3904, .T. ) ;
#13407 = LINE ( 'NONE', #11830, #3859 ) ;
#13408 = ORIENTED_EDGE ( 'NONE', *, *, #14155, .F. ) ;
#13409 = ORIENTED_EDGE ( 'NONE', *, *, #457, .F. ) ;
#13410 = PRODUCT ( '4-Bolt Mounting Plate', '4-Bolt Mounting Plate', '', ( #2363 ) ) ;
#13411 = VERTEX_POINT ( 'NONE', #9807 ) ;
#13412 = VECTOR ( 'NONE', #17257, 1000.000000000000000 ) ;
#13413 = ORIENTED_EDGE ( 'NONE', *, *, #6400, .T. ) ;
#13414 = LINE ( 'NONE', #16389, #1642 ) ;
#13415 = CARTESIAN_POINT ( 'NONE',  ( -71.24615306438076345, 123.0983361545637109, -167.1454815528550739 ) ) ;
#13416 = ORIENTED_EDGE ( 'NONE', *, *, #3732, .T. ) ;
#13417 = CARTESIAN_POINT ( 'NONE',  ( -68.99615306438117557, 5.151604338130305827, -15.00000000000001421 ) ) ;
#13418 = CARTESIAN_POINT ( 'NONE',  ( -68.12361985383350316, 84.22855780814606419, -47.49999999999999289 ) ) ;
#13419 = EDGE_LOOP ( 'NONE', ( #18010, #1091, #16021, #14394, #9436, #16757 ) ) ;
#13420 = DIRECTION ( 'NONE',  ( 1.000000000000000000, 0.000000000000000000, 0.000000000000000000 ) ) ;
#13421 = ORIENTED_EDGE ( 'NONE', *, *, #2984, .T. ) ;
#13422 = CIRCLE ( 'NONE', #4753, 4.600000000000006750 ) ;
#13423 = CARTESIAN_POINT ( 'NONE',  ( -70.27900850916093134, -2.213358015103445098, 15.00000000000008171 ) ) ;
#13424 = DIRECTION ( 'NONE',  ( 0.3420201433256891965, 0.9396926207859008784, -0.000000000000000000 ) ) ;
#13425 = ORIENTED_EDGE ( 'NONE', *, *, #10177, .T. ) ;
#13426 = CIRCLE ( 'NONE', #8657, 26.04359719766049608 ) ;
#13427 = DIRECTION ( 'NONE',  ( 0.000000000000000000, 5.551115123125748189E-17, 1.000000000000000000 ) ) ;
#13428 = CARTESIAN_POINT ( 'NONE',  ( -80.85270481228980088, -91.10977358899566525, -39.65137850708998002 ) ) ;
#13429 = ORIENTED_EDGE ( 'NONE', *, *, #10398, .F. ) ;
#13430 = ORIENTED_EDGE ( 'NONE', *, *, #10856, .T. ) ;
#13431 = VECTOR ( 'NONE', #4145, 1000.000000000000000 ) ;
#13433 = ADVANCED_FACE ( 'NONE', ( #8217 ), #8306, .T. ) ;
#13432 = CYLINDRICAL_SURFACE ( 'NONE', #4585, 12.49999999999999112 ) ;
#13434 = LINE ( 'NONE', #6415, #13835 ) ;
#13435 = ORIENTED_EDGE ( 'NONE', *, *, #489, .F. ) ;
#13436 = VECTOR ( 'NONE', #12764, 1000.000000000000000 ) ;
#13437 = SHAPE_DEFINITION_REPRESENTATION ( #10890, #15047 ) ;
#13438 = FACE_OUTER_BOUND ( 'NONE', #2596, .T. ) ;
#13439 =( NAMED_UNIT ( * ) PLANE_ANGLE_UNIT ( ) SI_UNIT ( $, .RADIAN. ) );
#13440 = LINE ( 'NONE', #899, #7277 ) ;
#13441 = CARTESIAN_POINT ( 'NONE',  ( -56.80760832784252301, 71.73152654333280509, -167.1454815528550739 ) ) ;
#13442 = VERTEX_POINT ( 'NONE', #14118 ) ;
#13443 = ADVANCED_FACE ( 'NONE', ( #1305 ), #11755, .T. ) ;
#13444 = DIRECTION ( 'NONE',  ( 1.000000000000000000, 0.000000000000000000, 0.000000000000000000 ) ) ;
#13445 = CARTESIAN_POINT ( 'NONE',  ( -112.5926225674731995, 50.58224449241410525, -35.00000000000000000 ) ) ;
#13446 = CARTESIAN_POINT ( 'NONE',  ( -57.08002265617300708, 84.22855780814606419, -167.1454815528550739 ) ) ;
#13447 = PLANE ( 'NONE',  #6026 ) ;
#13448 = DIRECTION ( 'NONE',  ( 0.000000000000000000, 1.000000000000000000, 0.000000000000000000 ) ) ;
#13449 = VERTEX_POINT ( 'NONE', #5938 ) ;
#13450 = DIRECTION ( 'NONE',  ( 0.000000000000000000, 0.000000000000000000, 1.000000000000000000 ) ) ;
#13451 = DIRECTION ( 'NONE',  ( -5.204170427930409450E-16, 0.000000000000000000, 1.000000000000000000 ) ) ;
#13452 = VECTOR ( 'NONE', #14844, 1000.000000000000000 ) ;
#13453 = ORIENTED_EDGE ( 'NONE', *, *, #1042, .T. ) ;
#13454 = CARTESIAN_POINT ( 'NONE',  ( -57.08002265617300708, 84.22855780814606419, -167.1454815528550739 ) ) ;
#13455 = VECTOR ( 'NONE', #14036, 1000.000000000000000 ) ;
#13456 = LINE ( 'NONE', #14933, #11677 ) ;
#13457 = VERTEX_POINT ( 'NONE', #5863 ) ;
#13458 = AXIS2_PLACEMENT_3D ( 'NONE', #1309, #17099, #8308 ) ;
#13459 = ORIENTED_EDGE ( 'NONE', *, *, #13630, .T. ) ;
#13460 = PLANE ( 'NONE',  #1315 ) ;
#13461 = CIRCLE ( 'NONE', #4205, 4.599999999999992539 ) ;
#13462 = ORIENTED_EDGE ( 'NONE', *, *, #4855, .F. ) ;
#13463 = CYLINDRICAL_SURFACE ( 'NONE', #6719, 3.999999999999996447 ) ;
#13464 = PLANE ( 'NONE',  #4858 ) ;
#13465 = VECTOR ( 'NONE', #8509, 1000.000000000000000 ) ;
#13466 = CARTESIAN_POINT ( 'NONE',  ( -70.27900850916091713, -2.213358015103439325, -15.00000000000001421 ) ) ;
#13467 = CARTESIAN_POINT ( 'NONE',  ( -68.99615306438111872, 20.24471173166267235, 15.00000000000006928 ) ) ;
#13468 = VECTOR ( 'NONE', #8586, 1000.000000000000000 ) ;
#13469 = EDGE_CURVE ( 'NONE', #9102, #5451, #1829, .T. ) ;
#13470 = DIRECTION ( 'NONE',  ( 0.9396926207859084279, 0.3420201433256686574, 4.890320548438448905E-16 ) ) ;
#13471 = FACE_OUTER_BOUND ( 'NONE', #10260, .T. ) ;
#13472 = VERTEX_POINT ( 'NONE', #10083 ) ;
#13473 = DIRECTION ( 'NONE',  ( -5.204170427930409450E-16, 0.000000000000000000, 1.000000000000000000 ) ) ;
#13474 = EDGE_CURVE ( 'NONE', #16963, #9640, #447, .T. ) ;
#13475 = CARTESIAN_POINT ( 'NONE',  ( -75.94240647281702650, 61.71752694572068521, -25.18301127684852858 ) ) ;
#13476 = DIRECTION ( 'NONE',  ( 0.000000000000000000, 0.000000000000000000, 1.000000000000000000 ) ) ;
#13477 = ORIENTED_EDGE ( 'NONE', *, *, #6404, .F. ) ;
#13478 = CYLINDRICAL_SURFACE ( 'NONE', #6727, 10.24900000000000055 ) ;
#13479 = LINE ( 'NONE', #7592, #858 ) ;
#13480 = VERTEX_POINT ( 'NONE', #6027 ) ;
#13481 = CIRCLE ( 'NONE', #6291, 10.24899999999999345 ) ;
#13482 = VECTOR ( 'NONE', #6554, 1000.000000000000000 ) ;
#13483 = EDGE_CURVE ( 'NONE', #4200, #7349, #13158, .T. ) ;
#13484 = ORIENTED_EDGE ( 'NONE', *, *, #5844, .T. ) ;
#13485 = EDGE_CURVE ( 'NONE', #12673, #4970, #8214, .T. ) ;
#13486 = CARTESIAN_POINT ( 'NONE',  ( -57.08002265617300708, 84.22855780814606419, -15.00000000000001421 ) ) ;
#13487 = FACE_OUTER_BOUND ( 'NONE', #178, .T. ) ;
#13488 = CARTESIAN_POINT ( 'NONE',  ( -57.08002265617300708, 84.22855780814606419, -167.1454815528550739 ) ) ;
#13489 = DIRECTION ( 'NONE',  ( 1.000000000000000000, 0.000000000000000000, 0.000000000000000000 ) ) ;
#13490 = VERTEX_POINT ( 'NONE', #7180 ) ;
#13491 = VECTOR ( 'NONE', #5543, 1000.000000000000114 ) ;
#13492 = CARTESIAN_POINT ( 'NONE',  ( -71.24615306438107609, 10.00100075456378157, 15.00000000000006928 ) ) ;
#13493 = FACE_OUTER_BOUND ( 'NONE', #17333, .T. ) ;
#13494 = VERTEX_POINT ( 'NONE', #17534 ) ;
#13495 = EDGE_CURVE ( 'NONE', #2512, #12063, #16127, .T. ) ;
#13496 = FACE_OUTER_BOUND ( 'NONE', #5698, .T. ) ;
#13497 = DIRECTION ( 'NONE',  ( 0.000000000000000000, -1.000000000000000000, 0.000000000000000000 ) ) ;
#13498 = DIRECTION ( 'NONE',  ( 0.000000000000000000, 0.000000000000000000, 1.000000000000000000 ) ) ;
#13499 = EDGE_CURVE ( 'NONE', #4091, #6989, #73, .T. ) ;
#13500 = CARTESIAN_POINT ( 'NONE',  ( -71.24615306438109030, 27.96168591522921076, -167.1454815528550739 ) ) ;
#13501 = AXIS2_PLACEMENT_3D ( 'NONE', #139, #11556, #13057 ) ;
#13502 = ORIENTED_EDGE ( 'NONE', *, *, #1138, .T. ) ;
#13503 = FACE_OUTER_BOUND ( 'NONE', #13757, .T. ) ;
#13504 = ORIENTED_EDGE ( 'NONE', *, *, #8928, .T. ) ;
#13505 = CARTESIAN_POINT ( 'NONE',  ( -71.24615306438086293, 91.68240965456375591, -167.1454815528550739 ) ) ;
#13506 = ORIENTED_EDGE ( 'NONE', *, *, #18331, .T. ) ;
#13507 = ADVANCED_FACE ( 'NONE', ( #7538 ), #249, .T. ) ;
#13508 = VECTOR ( 'NONE', #14715, 1000.000000000000227 ) ;
#13509 = ADVANCED_FACE ( 'NONE', ( #6120 ), #4715, .T. ) ;
#13510 = ORIENTED_EDGE ( 'NONE', *, *, #17104, .F. ) ;
#13511 = VECTOR ( 'NONE', #7272, 1000.000000000000000 ) ;
#13512 = VECTOR ( 'NONE', #631, 1000.000000000000000 ) ;
#13513 = EDGE_CURVE ( 'NONE', #2837, #18489, #4044, .T. ) ;
#13514 = EDGE_CURVE ( 'NONE', #5525, #6089, #15868, .T. ) ;
#13515 = CARTESIAN_POINT ( 'NONE',  ( -71.24615306438090556, 57.12489050456379402, 15.00000000000006928 ) ) ;
#13516 = ORIENTED_EDGE ( 'NONE', *, *, #3442, .F. ) ;
#13517 = DIRECTION ( 'NONE',  ( -0.000000000000000000, -0.000000000000000000, -1.000000000000000000 ) ) ;
#13518 = LINE ( 'NONE', #7902, #1930 ) ;
#13519 = VERTEX_POINT ( 'NONE', #8592 ) ;
#13520 = ADVANCED_FACE ( 'NONE', ( #14295 ), #7444, .T. ) ;
#13521 = VECTOR ( 'NONE', #17413, 1000.000000000000000 ) ;
#13522 = LINE ( 'NONE', #1921, #15580 ) ;
#13523 = ORIENTED_EDGE ( 'NONE', *, *, #9593, .T. ) ;
#13524 = CARTESIAN_POINT ( 'NONE',  ( 84.41679105416972106, 84.22855780814606419, 62.50000000000001421 ) ) ;
#13525 = CARTESIAN_POINT ( 'NONE',  ( -66.00585202009864361, 110.3988717985813395, 25.00000000000000355 ) ) ;
#13526 = AXIS2_PLACEMENT_3D ( 'NONE', #2587, #9875, #9784 ) ;
#13527 = CIRCLE ( 'NONE', #975, 3.999999999999989786 ) ;
#13528 = CARTESIAN_POINT ( 'NONE',  ( -38.09490121289055509, 73.26749283227019305, 102.5000000000000000 ) ) ;
#13529 = CARTESIAN_POINT ( 'NONE',  ( -68.99615306438080609, 108.2093059316626693, 15.00000000000006928 ) ) ;
#13530 = ORIENTED_EDGE ( 'NONE', *, *, #11735, .F. ) ;
#13531 = VECTOR ( 'NONE', #526, 1000.000000000000000 ) ;
#13532 = ORIENTED_EDGE ( 'NONE', *, *, #140, .F. ) ;
#13533 = CARTESIAN_POINT ( 'NONE',  ( -71.24615306438110451, 22.56737135456380372, -15.00000000000001421 ) ) ;
#13534 = DIRECTION ( 'NONE',  ( 1.000000000000000000, 0.000000000000000000, 3.771137991253934490E-16 ) ) ;
#13535 = ORIENTED_EDGE ( 'NONE', *, *, #8363, .F. ) ;
#13536 = VECTOR ( 'NONE', #9816, 1000.000000000000000 ) ;
#13537 = AXIS2_PLACEMENT_3D ( 'NONE', #17670, #10672, #6538 ) ;
#13538 = CYLINDRICAL_SURFACE ( 'NONE', #16282, 4.599999999999999645 ) ;
#13539 =( NAMED_UNIT ( * ) SI_UNIT ( $, .STERADIAN. ) SOLID_ANGLE_UNIT ( ) );
#13540 = CIRCLE ( 'NONE', #18339, 45.40389983439752086 ) ;
#13541 = CARTESIAN_POINT ( 'NONE',  ( -58.51182448057780050, 96.64628479562776420, -167.1454815528550739 ) ) ;
#13542 = LINE ( 'NONE', #12143, #10280 ) ;
#13543 = ORIENTED_EDGE ( 'NONE', *, *, #8937, .T. ) ;
#13544 = LINE ( 'NONE', #529, #9274 ) ;
#13545 = CARTESIAN_POINT ( 'NONE',  ( -71.24615306438103346, 47.70011255456374499, -167.1454815528550739 ) ) ;
#13546 = DIRECTION ( 'NONE',  ( 1.000000000000000000, 0.000000000000000000, 0.000000000000000000 ) ) ;
#13547 = DIRECTION ( 'NONE',  ( 0.000000000000000000, 1.000000000000000000, 0.000000000000000000 ) ) ;
#13548 = EDGE_LOOP ( 'NONE', ( #9459, #14550 ) ) ;
#13549 = CARTESIAN_POINT ( 'NONE',  ( -68.99615306438087714, 71.12504998813027157, 15.00000000000006928 ) ) ;
#13550 = CARTESIAN_POINT ( 'NONE',  ( -65.06546592763129411, -91.08423613455721579, -6.816485587782003001E-13 ) ) ;
#13551 = ORIENTED_EDGE ( 'NONE', *, *, #16444, .F. ) ;
#13552 = DIRECTION ( 'NONE',  ( 0.000000000000000000, 0.000000000000000000, 1.000000000000000000 ) ) ;
#13553 = AXIS2_PLACEMENT_3D ( 'NONE', #15410, #4090, #9984 ) ;
#13554 = CARTESIAN_POINT ( 'NONE',  ( -36.03642545851251100, 83.98232705807349419, 70.00000000000002842 ) ) ;
#13555 = ORIENTED_EDGE ( 'NONE', *, *, #11656, .F. ) ;
#13556 = TOROIDAL_SURFACE ( 'NONE', #16220, 7.372635429264279061, 4.962965561209096599 ) ;
#13557 = ORIENTED_EDGE ( 'NONE', *, *, #4121, .T. ) ;
#13558 = CARTESIAN_POINT ( 'NONE',  ( -70.85175816390371040, -141.5628872026273086, 18.23991632971911514 ) ) ;
#13559 = ORIENTED_EDGE ( 'NONE', *, *, #5806, .F. ) ;
#13560 = LINE ( 'NONE', #7748, #12407 ) ;
#13561 = DIRECTION ( 'NONE',  ( 0.3420201433256727097, 0.9396926207859069846, -0.000000000000000000 ) ) ;
#13562 = CARTESIAN_POINT ( 'NONE',  ( -66.00585202009801833, 57.88796029049324687, 25.00000000000000355 ) ) ;
#13563 = CARTESIAN_POINT ( 'NONE',  ( 94.09522336508815954, 84.22855780814606419, 69.87263542926429238 ) ) ;
#13564 = AXIS2_PLACEMENT_3D ( 'NONE', #17011, #8319, #7108 ) ;
#13565 = FACE_OUTER_BOUND ( 'NONE', #15880, .T. ) ;
#13566 = VECTOR ( 'NONE', #5152, 1000.000000000000000 ) ;
#13567 = CYLINDRICAL_SURFACE ( 'NONE', #7815, 3.999999999999989786 ) ;
#13568 = ORIENTED_EDGE ( 'NONE', *, *, #13340, .T. ) ;
#13569 = CARTESIAN_POINT ( 'NONE',  ( -71.24615306438079188, 94.82400230456380541, 15.00000000000006928 ) ) ;
#13570 = CARTESIAN_POINT ( 'NONE',  ( -98.90286936182243949, -96.08423613455721579, 10.65431531532547815 ) ) ;
#13571 = ORIENTED_EDGE ( 'NONE', *, *, #13983, .F. ) ;
#13572 = ADVANCED_FACE ( 'NONE', ( #4639 ), #11658, .T. ) ;
#13573 = AXIS2_PLACEMENT_3D ( 'NONE', #5072, #17990, #4983 ) ;
#13574 = CARTESIAN_POINT ( 'NONE',  ( -71.24615306438107609, 16.28418605456382906, 15.00000000000006928 ) ) ;
#13575 = DIRECTION ( 'NONE',  ( -1.000000000000000000, -4.062187864517847658E-15, 1.692578276882436442E-16 ) ) ;
#13576 = VERTEX_POINT ( 'NONE', #16044 ) ;
#13577 = CIRCLE ( 'NONE', #8244, 9.197489084949710403 ) ;
#13578 = CONICAL_SURFACE ( 'NONE', #11502, 12.29357405616490695, 0.1302312384721128480 ) ;
#13579 = AXIS2_PLACEMENT_3D ( 'NONE', #16849, #5430, #9836 ) ;
#13580 = ORIENTED_EDGE ( 'NONE', *, *, #1599, .F. ) ;
#13581 = PRODUCT_DEFINITION_CONTEXT ( 'detailed design', #15160, 'design' ) ;
#13582 = EDGE_CURVE ( 'NONE', #12161, #3245, #3158, .T. ) ;
#13583 = LINE ( 'NONE', #10865, #6401 ) ;
#13584 = DIRECTION ( 'NONE',  ( -1.000000000000000000, 0.000000000000000000, 0.000000000000000000 ) ) ;
#13585 = DIRECTION ( 'NONE',  ( 0.9396926207859069846, 0.3420201433256723766, 4.890320548438442003E-16 ) ) ;
#13586 = CARTESIAN_POINT ( 'NONE',  ( -76.06514409945376087, 73.26749283226919829, 102.5000000000000000 ) ) ;
#13587 = AXIS2_PLACEMENT_3D ( 'NONE', #8640, #1532, #7239 ) ;
#13588 = EDGE_LOOP ( 'NONE', ( #18200, #12612, #14764, #9118 ) ) ;
#13589 = DIRECTION ( 'NONE',  ( 0.3420201433256724322, 0.9396926207859070956, -0.000000000000000000 ) ) ;
#13590 = DIRECTION ( 'NONE',  ( -1.000000000000000000, 0.000000000000000000, 0.000000000000000000 ) ) ;
#13591 = ORIENTED_EDGE ( 'NONE', *, *, #3446, .F. ) ;
#13592 = VECTOR ( 'NONE', #3411, 1000.000000000000000 ) ;
#13593 = CARTESIAN_POINT ( 'NONE',  ( -63.16290507965269541, 75.97988867778799715, -167.1454815528550739 ) ) ;
#13594 = CYLINDRICAL_SURFACE ( 'NONE', #17962, 4.999999999999997335 ) ;
#13595 = CARTESIAN_POINT ( 'NONE',  ( -76.98456221794718601, 91.05880801963004956, 59.39221631177008476 ) ) ;
#13596 = DIRECTION ( 'NONE',  ( 0.9396926207859157554, 0.3420201433256481738, 4.890320548438487362E-16 ) ) ;
#13597 = AXIS2_PLACEMENT_3D ( 'NONE', #15341, #16445, #12253 ) ;
#13598 = VERTEX_POINT ( 'NONE', #8673 ) ;
#13599 = CONICAL_SURFACE ( 'NONE', #1365, 6.500000000000039968, 1.047197551196600296 ) ;
#13600 = CARTESIAN_POINT ( 'NONE',  ( 5.299999999999998934, 3.608224830031735584E-16, 6.499999999999999112 ) ) ;
#13601 = VERTEX_POINT ( 'NONE', #7275 ) ;
#13602 = LINE ( 'NONE', #16385, #533 ) ;
#13603 = VERTEX_POINT ( 'NONE', #334 ) ;
#13604 = ORIENTED_EDGE ( 'NONE', *, *, #14181, .T. ) ;
#13605 = VECTOR ( 'NONE', #16888, 1000.000000000000000 ) ;
#13606 = EDGE_CURVE ( 'NONE', #14578, #15061, #17267, .T. ) ;
#13607 = EDGE_CURVE ( 'NONE', #5337, #14175, #801, .T. ) ;
#13608 = TOROIDAL_SURFACE ( 'NONE', #9133, 10.65431531532568243, 5.000000000000000000 ) ;
#13609 = EDGE_CURVE ( 'NONE', #16233, #5685, #11515, .T. ) ;
#13610 = LINE ( 'NONE', #10616, #10831 ) ;
#13611 = EDGE_LOOP ( 'NONE', ( #10477, #16717, #4906, #2200 ) ) ;
#13612 = CARTESIAN_POINT ( 'NONE',  ( -71.24615306438080609, 115.9262801152292042, -15.00000000000001421 ) ) ;
#13613 = FACE_OUTER_BOUND ( 'NONE', #1376, .T. ) ;
#13614 = ORIENTED_EDGE ( 'NONE', *, *, #12149, .F. ) ;
#13615 = CARTESIAN_POINT ( 'NONE',  ( -70.06856178257680767, 110.5691553257988460, 22.35917033480641791 ) ) ;
#13616 = EDGE_CURVE ( 'NONE', #2018, #2837, #17465, .T. ) ;
#13617 = VERTEX_POINT ( 'NONE', #17727 ) ;
#13618 = EDGE_CURVE ( 'NONE', #14603, #11466, #4910, .T. ) ;
#13619 = DIRECTION ( 'NONE',  ( -0.000000000000000000, -0.000000000000000000, -1.000000000000000000 ) ) ;
#13620 = CARTESIAN_POINT ( 'NONE',  ( -71.24615306438117557, 2.828944715229236628, 15.00000000000006928 ) ) ;
#13621 = ORIENTED_EDGE ( 'NONE', *, *, #12482, .T. ) ;
#13622 = EDGE_CURVE ( 'NONE', #9739, #5564, #18063, .T. ) ;
#13623 = FACE_BOUND ( 'NONE', #16579, .T. ) ;
#13624 = EDGE_CURVE ( 'NONE', #5660, #8650, #6403, .T. ) ;
#13625 = CARTESIAN_POINT ( 'NONE',  ( -68.99615306438080609, 108.8241617881302545, -167.1454815528550739 ) ) ;
#13626 = ORIENTED_EDGE ( 'NONE', *, *, #3441, .T. ) ;
#13627 = EDGE_LOOP ( 'NONE', ( #5873, #6236, #2631, #13135 ) ) ;
#13628 = EDGE_CURVE ( 'NONE', #14282, #797, #16503, .T. ) ;
#13629 = EDGE_CURVE ( 'NONE', #10960, #12217, #3318, .T. ) ;
#13630 = EDGE_CURVE ( 'NONE', #6089, #7142, #9413, .T. ) ;
#13631 = EDGE_LOOP ( 'NONE', ( #11524, #3081, #2366, #7698 ) ) ;
#13632 = LINE ( 'NONE', #9421, #7282 ) ;
#13633 = FACE_OUTER_BOUND ( 'NONE', #5862, .T. ) ;
#13634 = ORIENTED_EDGE ( 'NONE', *, *, #3423, .F. ) ;
#13635 = CARTESIAN_POINT ( 'NONE',  ( -70.71978124295708312, -96.08423613455721579, 28.18308811886538479 ) ) ;
#13636 = DIRECTION ( 'NONE',  ( -1.000000000000000000, -0.000000000000000000, -0.000000000000000000 ) ) ;
#13637 = DIRECTION ( 'NONE',  ( 0.000000000000000000, 0.000000000000000000, 1.000000000000000000 ) ) ;
#13638 = FACE_OUTER_BOUND ( 'NONE', #17598, .T. ) ;
#13639 = ORIENTED_EDGE ( 'NONE', *, *, #11525, .F. ) ;
#13640 = LINE ( 'NONE', #12330, #5696 ) ;
#13641 = DIRECTION ( 'NONE',  ( 1.000000000000000000, -0.000000000000000000, -0.000000000000000000 ) ) ;
#13642 = CARTESIAN_POINT ( 'NONE',  ( -71.24615306438114715, 16.28418605456380419, -167.1454815528550739 ) ) ;
#13643 = DIRECTION ( 'NONE',  ( 0.000000000000000000, 0.000000000000000000, 1.000000000000000000 ) ) ;
#13644 = VERTEX_POINT ( 'NONE', #12314 ) ;
#13645 = ADVANCED_FACE ( 'NONE', ( #7991 ), #4995, .T. ) ;
#13646 = FACE_OUTER_BOUND ( 'NONE', #6545, .T. ) ;
#13647 = CARTESIAN_POINT ( 'NONE',  ( -70.71978124295668522, -91.08423613455721579, -28.18308811886538479 ) ) ;
#13648 = EDGE_CURVE ( 'NONE', #3936, #565, #14214, .T. ) ;
#13649 = ORIENTED_EDGE ( 'NONE', *, *, #6750, .T. ) ;
#13650 = DIRECTION ( 'NONE',  ( 0.000000000000000000, 0.000000000000000000, 1.000000000000000000 ) ) ;
#13651 = CARTESIAN_POINT ( 'NONE',  ( -36.07112927697242100, 82.99614312904145663, 69.90220970626739927 ) ) ;
#13652 = ORIENTED_EDGE ( 'NONE', *, *, #5841, .F. ) ;
#13653 = EDGE_LOOP ( 'NONE', ( #15716, #17579, #11801, #16339, #981, #13087, #7593, #4455 ) ) ;
#13654 = CARTESIAN_POINT ( 'NONE',  ( -57.08002265617300708, 84.22855780814606419, -47.50000000000000000 ) ) ;
#13655 = ORIENTED_EDGE ( 'NONE', *, *, #16227, .T. ) ;
#13656 = CARTESIAN_POINT ( 'NONE',  ( -67.59262256747315689, 56.80567558672318285, -15.00000000000000711 ) ) ;
#13657 = CARTESIAN_POINT ( 'NONE',  ( -72.31238267408940601, 59.11671001647612655, 22.54839013747459120 ) ) ;
#13658 = LINE ( 'NONE', #10843, #6992 ) ;
#13659 = CARTESIAN_POINT ( 'NONE',  ( -57.08002265617302839, 27.37185818390810965, 92.50000000000000000 ) ) ;
#13660 = CARTESIAN_POINT ( 'NONE',  ( -107.5926225674731853, 110.5691553257988460, -30.35917033480641081 ) ) ;
#13661 = DIRECTION ( 'NONE',  ( 0.000000000000000000, 0.000000000000000000, 1.000000000000000000 ) ) ;
#13662 = FACE_OUTER_BOUND ( 'NONE', #8113, .T. ) ;
#13663 = EDGE_LOOP ( 'NONE', ( #18248, #12052, #12491, #7984 ) ) ;
#13664 = ADVANCED_FACE ( 'NONE', ( #13623, #12210, #14730 ), #10527, .F. ) ;
#13665 = DIRECTION ( 'NONE',  ( -0.000000000000000000, -0.000000000000000000, 1.000000000000000000 ) ) ;
#13666 = CARTESIAN_POINT ( 'NONE',  ( -71.24615306438076345, 119.9567435045637609, -15.00000000000001421 ) ) ;
#13667 = ORIENTED_EDGE ( 'NONE', *, *, #2650, .T. ) ;
#13668 = CARTESIAN_POINT ( 'NONE',  ( -107.5926225674731853, 60.58224449241411946, -25.00000000000000000 ) ) ;
#13669 = DIRECTION ( 'NONE',  ( 0.000000000000000000, 0.000000000000000000, 1.000000000000000000 ) ) ;
#13670 = ORIENTED_EDGE ( 'NONE', *, *, #7436, .F. ) ;
#13671 = ORIENTED_EDGE ( 'NONE', *, *, #6814, .T. ) ;
#13672 = FACE_BOUND ( 'NONE', #6096, .T. ) ;
#13673 = CARTESIAN_POINT ( 'NONE',  ( -51.85133027979232878, 95.58244595420329404, 15.00000000000006928 ) ) ;
#13674 = DIRECTION ( 'NONE',  ( -1.000000000000000000, 0.000000000000000000, 1.387778780781445182E-16 ) ) ;
#13675 = EDGE_CURVE ( 'NONE', #11552, #15366, #9105, .T. ) ;
#13676 = DIRECTION ( 'NONE',  ( -0.9396926207859069846, 0.3420201433256723766, -4.890320548438442003E-16 ) ) ;
#13677 = CARTESIAN_POINT ( 'NONE',  ( -57.08002265617300708, 84.22855780814606419, -15.00000000000001421 ) ) ;
#13678 = CARTESIAN_POINT ( 'NONE',  ( 0.4033376246892572681, 7.198601258566914574, -0.5316568767329080680 ) ) ;
#13679 = ORIENTED_EDGE ( 'NONE', *, *, #6295, .F. ) ;
#13680 = DIRECTION ( 'NONE',  ( 0.000000000000000000, 0.000000000000000000, 1.000000000000000000 ) ) ;
#13681 = CARTESIAN_POINT ( 'NONE',  ( -57.08002265617300708, 84.22855780814606419, -15.00000000000000711 ) ) ;
#13683 = VERTEX_POINT ( 'NONE', #12030 ) ;
#13682 = DIRECTION ( 'NONE',  ( 1.000000000000000000, 0.000000000000000000, 0.000000000000000000 ) ) ;
#13684 = CARTESIAN_POINT ( 'NONE',  ( -109.8630080638467064, -91.08423613455721579, 10.52500441287563326 ) ) ;
#13685 = VERTEX_POINT ( 'NONE', #6202 ) ;
#13686 = PLANE ( 'NONE',  #17031 ) ;
#13687 = ORIENTED_EDGE ( 'NONE', *, *, #5146, .F. ) ;
#13688 = DIRECTION ( 'NONE',  ( -1.000000000000000000, -0.000000000000000000, -0.000000000000000000 ) ) ;
#13689 = ORIENTED_EDGE ( 'NONE', *, *, #14221, .T. ) ;
#13690 = ORIENTED_EDGE ( 'NONE', *, *, #3512, .T. ) ;
#13691 = DIRECTION ( 'NONE',  ( 1.000000000000000000, 2.062304371594500740E-16, -0.000000000000000000 ) ) ;
#13692 = TOROIDAL_SURFACE ( 'NONE', #5634, 10.65431531532567888, 5.000000000000000000 ) ;
#13693 = CARTESIAN_POINT ( 'NONE',  ( 4.699999999999995737, 3.752776749732435135, 6.499999999999981348 ) ) ;
#13694 = EDGE_LOOP ( 'NONE', ( #3836, #14854, #2333, #7634 ) ) ;
#13695 = ADVANCED_FACE ( 'NONE', ( #7911 ), #9219, .T. ) ;
#13696 = CARTESIAN_POINT ( 'NONE',  ( -70.27900850916093134, -2.213358015103445098, -167.1454815528550739 ) ) ;
#13697 = DIRECTION ( 'NONE',  ( 0.9396926207859069846, 0.3420201433256723766, -1.086737899652988166E-16 ) ) ;
#13698 = ORIENTED_EDGE ( 'NONE', *, *, #3280, .T. ) ;
#13699 = FILL_AREA_STYLE_COLOUR ( '', #16754 ) ;
#13700 = DIRECTION ( 'NONE',  ( 0.000000000000000000, 0.000000000000000000, 1.000000000000000000 ) ) ;
#13701 = ORIENTED_EDGE ( 'NONE', *, *, #14067, .T. ) ;
#13702 = CARTESIAN_POINT ( 'NONE',  ( -73.18550356302633020, 108.7913366739104646, -22.76494920255247578 ) ) ;
#13703 = CARTESIAN_POINT ( 'NONE',  ( -71.24615306438117557, 3.717815454563750954, 15.00000000000006928 ) ) ;
#13704 = EDGE_LOOP ( 'NONE', ( #3040, #17691, #10416, #970 ) ) ;
#13705 = EDGE_CURVE ( 'NONE', #3974, #13190, #4911, .T. ) ;
#13706 = DIRECTION ( 'NONE',  ( -2.062304371594500494E-16, 1.000000000000000000, 0.000000000000000000 ) ) ;
#13707 = VECTOR ( 'NONE', #5045, 1000.000000000000000 ) ;
#13708 = DIRECTION ( 'NONE',  ( -1.000000000000000000, 0.000000000000000000, 0.000000000000000000 ) ) ;
#13709 = EDGE_LOOP ( 'NONE', ( #5535, #16043, #275, #17939 ) ) ;
#13710 = EDGE_CURVE ( 'NONE', #1317, #10905, #7813, .T. ) ;
#13711 = CARTESIAN_POINT ( 'NONE',  ( 5.699999999999996625, 0.000000000000000000, 0.000000000000000000 ) ) ;
#13712 = LINE ( 'NONE', #2296, #10540 ) ;
#13713 = EDGE_CURVE ( 'NONE', #3860, #15763, #3591, .T. ) ;
#13714 = ORIENTED_EDGE ( 'NONE', *, *, #4838, .F. ) ;
#13715 = DIRECTION ( 'NONE',  ( 0.000000000000000000, 0.000000000000000000, 1.000000000000000000 ) ) ;
#13716 = CARTESIAN_POINT ( 'NONE',  ( -7.398807083024507847, 21.35709021097153482, 42.97347408463063090 ) ) ;
#13717 = VECTOR ( 'NONE', #3224, 1000.000000000000000 ) ;
#13718 = DIRECTION ( 'NONE',  ( 0.000000000000000000, -1.000000000000000000, 0.000000000000000000 ) ) ;
#13719 = ORIENTED_EDGE ( 'NONE', *, *, #17610, .T. ) ;
#13720 = DIRECTION ( 'NONE',  ( 0.000000000000000000, 0.000000000000000000, 1.000000000000000000 ) ) ;
#13721 = AXIS2_PLACEMENT_3D ( 'NONE', #336, #6028, #11756 ) ;
#13722 = LINE ( 'NONE', #12333, #6426 ) ;
#13723 = DIRECTION ( 'NONE',  ( 1.000000000000000000, 0.000000000000000000, 5.077734830647302671E-16 ) ) ;
#13724 = VERTEX_POINT ( 'NONE', #3877 ) ;
#13725 = ADVANCED_BREP_SHAPE_REPRESENTATION ( '', ( #314, #16217 ), #2194 ) ;
#13726 = EDGE_CURVE ( 'NONE', #8524, #1462, #15401, .T. ) ;
#13727 = ADVANCED_FACE ( 'NONE', ( #15293 ), #5370, .F. ) ;
#13728 = ADVANCED_FACE ( 'NONE', ( #15488, #1614 ), #3792, .T. ) ;
#13729 = DIRECTION ( 'NONE',  ( 1.000000000000000000, 0.000000000000000000, 0.000000000000000000 ) ) ;
#13730 = CARTESIAN_POINT ( 'NONE',  ( -60.06546592763143622, -91.08423613455721579, 38.97384619189705290 ) ) ;
#13731 = ORIENTED_EDGE ( 'NONE', *, *, #5154, .F. ) ;
#13732 = PLANE ( 'NONE',  #13755 ) ;
#13733 = CARTESIAN_POINT ( 'NONE',  ( -36.26589399568750594, 81.12099773066753983, 69.33028675349314085 ) ) ;
#13734 = ORIENTED_EDGE ( 'NONE', *, *, #8924, .T. ) ;
#13735 = AXIS2_PLACEMENT_3D ( 'NONE', #6098, #11907, #9201 ) ;
#13736 = EDGE_LOOP ( 'NONE', ( #6642, #8292, #8119, #18510, #2948, #6136, #399, #7109, #8652, #8286, #11045 ) ) ;
#13737 = EDGE_CURVE ( 'NONE', #1908, #5425, #11222, .T. ) ;
#13738 = VECTOR ( 'NONE', #4439, 1000.000000000000000 ) ;
#13739 = DIRECTION ( 'NONE',  ( 0.000000000000000000, 0.000000000000000000, -1.000000000000000000 ) ) ;
#13740 = EDGE_LOOP ( 'NONE', ( #15448, #995, #11309, #4963 ) ) ;
#13741 = EDGE_CURVE ( 'NONE', #8485, #15227, #11530, .T. ) ;
#13742 = CARTESIAN_POINT ( 'NONE',  ( -71.24615306438114715, 15.39531531522927921, -15.00000000000001421 ) ) ;
#13743 = CARTESIAN_POINT ( 'NONE',  ( -73.88125023881575260, 60.13841621731533849, 23.04531203040799525 ) ) ;
#13744 = EDGE_CURVE ( 'NONE', #14175, #14482, #12419, .T. ) ;
#13745 = CARTESIAN_POINT ( 'NONE',  ( -66.26741375599719674, 58.64497179233082846, -28.00000000000000000 ) ) ;
#13746 = CARTESIAN_POINT ( 'NONE',  ( -71.24615306438097662, 60.26648315456372984, -167.1454815528550739 ) ) ;
#13747 = DIRECTION ( 'NONE',  ( 0.000000000000000000, 0.000000000000000000, 1.000000000000000000 ) ) ;
#13748 = CARTESIAN_POINT ( 'NONE',  ( -62.11705611183893438, 93.78931001713317528, 15.00000000000006928 ) ) ;
#13749 = CARTESIAN_POINT ( 'NONE',  ( -57.08002265617300708, 84.22855780814606419, -15.00000000000001421 ) ) ;
#13750 = VERTEX_POINT ( 'NONE', #14092 ) ;
#13751 = VECTOR ( 'NONE', #1350, 999.9999999999998863 ) ;
#13752 = ADVANCED_FACE ( 'NONE', ( #8191 ), #7324, .T. ) ;
#13753 = DIRECTION ( 'NONE',  ( 0.3420201433256649937, 0.9396926207859097602, -0.000000000000000000 ) ) ;
#13754 = VECTOR ( 'NONE', #18240, 1000.000000000000000 ) ;
#13755 = AXIS2_PLACEMENT_3D ( 'NONE', #10939, #15034, #5220 ) ;
#13756 = LINE ( 'NONE', #5041, #7770 ) ;
#13757 = EDGE_LOOP ( 'NONE', ( #18023, #17273, #520, #11529 ) ) ;
#13758 = CARTESIAN_POINT ( 'NONE',  ( -26.78696867915027724, -93.09900487505512956, -6.628864488196836824 ) ) ;
#13759 = PLANE ( 'NONE',  #16377 ) ;
#13760 = ORIENTED_EDGE ( 'NONE', *, *, #3106, .F. ) ;
#13761 = ORIENTED_EDGE ( 'NONE', *, *, #14261, .T. ) ;
#13762 = VECTOR ( 'NONE', #7015, 1000.000000000000000 ) ;
#13763 = CIRCLE ( 'NONE', #15844, 26.04359719766049608 ) ;
#13764 = ORIENTED_EDGE ( 'NONE', *, *, #14625, .F. ) ;
#13765 = AXIS2_PLACEMENT_3D ( 'NONE', #15209, #4183, #1297 ) ;
#13766 = VECTOR ( 'NONE', #12617, 1000.000000000000000 ) ;
#13767 = DIRECTION ( 'NONE',  ( -1.000000000000000000, -0.000000000000000000, -0.000000000000000000 ) ) ;
#13768 = CARTESIAN_POINT ( 'NONE',  ( -71.24615306438109030, 24.82009326522924297, -15.00000000000001421 ) ) ;
#13769 = DIRECTION ( 'NONE',  ( 1.000000000000000000, 0.000000000000000000, 5.077734830647306615E-16 ) ) ;
#13770 = CARTESIAN_POINT ( 'NONE',  ( -92.59262256747321373, 117.8748711238780515, -25.00000000000000000 ) ) ;
#13771 = LINE ( 'NONE', #13492, #886 ) ;
#13772 = CARTESIAN_POINT ( 'NONE',  ( -75.86129610575210336, 106.8071537307722991, 25.00000000000000355 ) ) ;
#13773 = ORIENTED_EDGE ( 'NONE', *, *, #2298, .F. ) ;
#13774 = CYLINDRICAL_SURFACE ( 'NONE', #6929, 6.500000000000039968 ) ;
#13775 = DIRECTION ( 'NONE',  ( 0.000000000000000000, 1.000000000000000000, -5.906678677474559343E-17 ) ) ;
#13777 = VERTEX_POINT ( 'NONE', #211 ) ;
#13776 = FACE_OUTER_BOUND ( 'NONE', #15305, .T. ) ;
#13778 = VECTOR ( 'NONE', #3482, 1000.000000000000000 ) ;
#13779 = DIRECTION ( 'NONE',  ( 0.000000000000000000, 0.000000000000000000, 1.000000000000000000 ) ) ;
#13780 = DIRECTION ( 'NONE',  ( 0.3420201433256686574, -0.9396926207859084279, 0.000000000000000000 ) ) ;
#13781 = ORIENTED_EDGE ( 'NONE', *, *, #1407, .T. ) ;
#13782 = AXIS2_PLACEMENT_3D ( 'NONE', #17263, #67, #5764 ) ;
#13783 = AXIS2_PLACEMENT_3D ( 'NONE', #15180, #3582, #979 ) ;
#13784 = CARTESIAN_POINT ( 'NONE',  ( -3.930119462002491844E-14, -111.0842361345572158, 5.654315315326165603 ) ) ;
#13785 = ORIENTED_EDGE ( 'NONE', *, *, #18207, .F. ) ;
#13786 = PRODUCT_DEFINITION ( 'UNKNOWN', '', #7580, #10962 ) ;
#13787 = EDGE_LOOP ( 'NONE', ( #18361, #5758, #2119, #18136 ) ) ;
#13788 = AXIS2_PLACEMENT_3D ( 'NONE', #11902, #5997, #6091 ) ;
#13789 = LINE ( 'NONE', #4072, #12021 ) ;
#13790 = VERTEX_POINT ( 'NONE', #5899 ) ;
#13791 = CIRCLE ( 'NONE', #1833, 10.38004356723770627 ) ;
#13792 = VECTOR ( 'NONE', #3267, 1000.000000000000000 ) ;
#13793 = LINE ( 'NONE', #5182, #2127 ) ;
#13794 = CARTESIAN_POINT ( 'NONE',  ( -68.99615306438066398, 130.8153103381302458, 15.00000000000006928 ) ) ;
#13795 = ORIENTED_EDGE ( 'NONE', *, *, #13268, .T. ) ;
#13796 = LINE ( 'NONE', #9407, #1812 ) ;
#13797 = DIRECTION ( 'NONE',  ( 0.000000000000000000, 0.000000000000000000, 1.000000000000000000 ) ) ;
#13798 = LINE ( 'NONE', #12307, #17096 ) ;
#13799 = EDGE_LOOP ( 'NONE', ( #8941, #1619, #17082, #8242 ) ) ;
#13800 = CARTESIAN_POINT ( 'NONE',  ( -75.86088625105277572, 106.8078580376686944, -24.98227212054766611 ) ) ;
#13801 = CARTESIAN_POINT ( 'NONE',  ( -48.99724571598702738, 77.92691374209489652, -167.1454815528550739 ) ) ;
#13802 = ORIENTED_EDGE ( 'NONE', *, *, #4597, .T. ) ;
#13803 = AXIS2_PLACEMENT_3D ( 'NONE', #13415, #16589, #9027 ) ;
#13804 = DIRECTION ( 'NONE',  ( 0.9396926207859158664, 0.3420201433256481738, -1.086737899652998397E-16 ) ) ;
#13805 = CARTESIAN_POINT ( 'NONE',  ( 4.699999999999995737, 3.752776749732435135, 6.499999999999981348 ) ) ;
#13806 = CIRCLE ( 'NONE', #5738, 6.500000000000039968 ) ;
#13807 = VERTEX_POINT ( 'NONE', #16978 ) ;
#13808 = ORIENTED_EDGE ( 'NONE', *, *, #6041, .T. ) ;
#13809 = CARTESIAN_POINT ( 'NONE',  ( 94.09522336508815954, 84.22855780814606419, 62.50000000000001421 ) ) ;
#13810 = DIRECTION ( 'NONE',  ( -1.000000000000000000, 0.000000000000000000, 0.000000000000000000 ) ) ;
#13811 = AXIS2_PLACEMENT_3D ( 'NONE', #15385, #11180, #8176 ) ;
#13812 = ORIENTED_EDGE ( 'NONE', *, *, #8914, .F. ) ;
#13813 = EDGE_CURVE ( 'NONE', #1187, #6109, #16784, .T. ) ;
#13814 = LINE ( 'NONE', #6993, #17606 ) ;
#13815 = CARTESIAN_POINT ( 'NONE',  ( -77.78561374552398888, 80.46558623543624833, 56.00764281523724009 ) ) ;
#13816 = CARTESIAN_POINT ( 'NONE',  ( -92.59262256747321373, 117.8748711238780373, 35.00000000000000000 ) ) ;
#13817 = CARTESIAN_POINT ( 'NONE',  ( 113.3630170098442989, -111.0842361345572158, 3.000000000000000000 ) ) ;
#13818 = VERTEX_POINT ( 'NONE', #6979 ) ;
#13819 = FACE_OUTER_BOUND ( 'NONE', #5586, .T. ) ;
#13820 = VECTOR ( 'NONE', #2069, 1000.000000000000000 ) ;
#13821 = CIRCLE ( 'NONE', #7255, 4.599999999999992539 ) ;
#13822 = DIRECTION ( 'NONE',  ( 0.000000000000000000, 0.000000000000000000, 1.000000000000000000 ) ) ;
#13823 = CARTESIAN_POINT ( 'NONE',  ( -0.2208807544345702534, 8.409232685097855153, -47.97696181894473710 ) ) ;
#13824 = DIRECTION ( 'NONE',  ( -5.204170427930409450E-16, 0.000000000000000000, 1.000000000000000000 ) ) ;
#13825 = ORIENTED_EDGE ( 'NONE', *, *, #13255, .T. ) ;
#13826 = PLANE ( 'NONE',  #6405 ) ;
#13827 = CARTESIAN_POINT ( 'NONE',  ( -60.32591256472624508, -91.08930925317537231, 39.31392926885263250 ) ) ;
#13828 = EDGE_CURVE ( 'NONE', #12168, #15032, #3155, .T. ) ;
#13829 = VERTEX_POINT ( 'NONE', #8290 ) ;
#13830 = AXIS2_PLACEMENT_3D ( 'NONE', #13586, #17870, #11987 ) ;
#13831 = LINE ( 'NONE', #3621, #11957 ) ;
#13832 = ORIENTED_EDGE ( 'NONE', *, *, #5576, .T. ) ;
#13833 = ORIENTED_EDGE ( 'NONE', *, *, #14235, .T. ) ;
#13834 = VECTOR ( 'NONE', #10948, 1000.000000000000000 ) ;
#13835 = VECTOR ( 'NONE', #10537, 1000.000000000000000 ) ;
#13836 = CIRCLE ( 'NONE', #3373, 4.999999999999993783 ) ;
#13837 = DIRECTION ( 'NONE',  ( 0.000000000000000000, 1.000000000000000000, -0.000000000000000000 ) ) ;
#13838 = EDGE_CURVE ( 'NONE', #7151, #11452, #15191, .T. ) ;
#13839 = VERTEX_POINT ( 'NONE', #1098 ) ;
#13840 = EDGE_CURVE ( 'NONE', #8753, #12673, #15708, .T. ) ;
#13841 = DIRECTION ( 'NONE',  ( 0.000000000000000000, 0.000000000000000000, 1.000000000000000000 ) ) ;
#13842 = DIRECTION ( 'NONE',  ( 0.3420201433256854218, 0.9396926207859023217, -0.000000000000000000 ) ) ;
#13843 = CARTESIAN_POINT ( 'NONE',  ( -65.94558993203320085, 89.37090336996871542, 15.00000000000006928 ) ) ;
#13844 = AXIS2_PLACEMENT_3D ( 'NONE', #15414, #12520, #4094 ) ;
#13845 = DIRECTION ( 'NONE',  ( 0.3420201433256929158, 0.9396926207858996571, -0.000000000000000000 ) ) ;
#13846 = DIRECTION ( 'NONE',  ( 1.000000000000000000, 0.000000000000000000, 0.000000000000000000 ) ) ;
#13847 = PLANE ( 'NONE',  #4622 ) ;
#13848 = LINE ( 'NONE', #16544, #16489 ) ;
#13849 = ORIENTED_EDGE ( 'NONE', *, *, #10630, .T. ) ;
#13850 = FACE_OUTER_BOUND ( 'NONE', #16046, .T. ) ;
#13851 = AXIS2_PLACEMENT_3D ( 'NONE', #14102, #2876, #16985 ) ;
#13852 = AXIS2_PLACEMENT_3D ( 'NONE', #15618, #14226, #5684 ) ;
#13853 = CARTESIAN_POINT ( 'NONE',  ( -62.30871503255384170, 95.58244595420320877, 15.00000000000006928 ) ) ;
#13854 = EDGE_CURVE ( 'NONE', #5784, #17050, #18300, .T. ) ;
#13855 = VERTEX_POINT ( 'NONE', #12509 ) ;
#13856 = DIRECTION ( 'NONE',  ( -1.000000000000000000, 0.000000000000000000, 0.000000000000000000 ) ) ;
#13857 = PLANE ( 'NONE',  #7423 ) ;
#13858 = EDGE_CURVE ( 'NONE', #10943, #12606, #18202, .T. ) ;
#13859 = EDGE_LOOP ( 'NONE', ( #6007, #12404, #7330, #11521 ) ) ;
#13860 = EDGE_CURVE ( 'NONE', #10561, #6934, #11197, .T. ) ;
#13861 = ORIENTED_EDGE ( 'NONE', *, *, #16791, .F. ) ;
#13862 = ORIENTED_EDGE ( 'NONE', *, *, #15449, .F. ) ;
#13863 = ADVANCED_FACE ( 'NONE', ( #12703 ), #4085, .T. ) ;
#13864 = ADVANCED_FACE ( 'NONE', ( #11292 ), #1979, .T. ) ;
#13865 = AXIS2_PLACEMENT_3D ( 'NONE', #3716, #16327, #6504 ) ;
#13866 = VECTOR ( 'NONE', #8578, 999.9999999999998863 ) ;
#13867 = LINE ( 'NONE', #1059, #8530 ) ;
#13868 = DIRECTION ( 'NONE',  ( -0.000000000000000000, -1.000000000000000000, -0.000000000000000000 ) ) ;
#13869 = CARTESIAN_POINT ( 'NONE',  ( -71.24615306438076345, 125.3510580652292248, -167.1454815528550739 ) ) ;
#13870 = CARTESIAN_POINT ( 'NONE',  ( -68.99615306438089135, 80.54982793813027797, -167.1454815528550739 ) ) ;
#13871 = FACE_OUTER_BOUND ( 'NONE', #13220, .T. ) ;
#13872 = DIRECTION ( 'NONE',  ( 0.000000000000000000, 0.000000000000000000, 1.000000000000000000 ) ) ;
#13873 = APPLICATION_CONTEXT ( 'automotive_design' ) ;
#13874 = EDGE_LOOP ( 'NONE', ( #9749, #15669, #12554, #6253, #14745 ) ) ;
#13875 = FACE_OUTER_BOUND ( 'NONE', #16301, .T. ) ;
#13876 = DIRECTION ( 'NONE',  ( 0.000000000000000000, 0.000000000000000000, 1.000000000000000000 ) ) ;
#13878 = EDGE_LOOP ( 'NONE', ( #2726, #12753, #1641, #12184 ) ) ;
#13877 = CARTESIAN_POINT ( 'NONE',  ( -77.26539832087783566, 90.18382313193714594, 67.08526386498388661 ) ) ;
#13879 = LINE ( 'NONE', #14061, #1573 ) ;
#13880 = LINE ( 'NONE', #15373, #12859 ) ;
#13881 = ORIENTED_EDGE ( 'NONE', *, *, #12712, .F. ) ;
#13882 = CONICAL_SURFACE ( 'NONE', #8195, 4.025000000000000355, 0.7853981633974482790 ) ;
#13883 = AXIS2_PLACEMENT_3D ( 'NONE', #681, #6559, #9468 ) ;
#13884 = AXIS2_PLACEMENT_3D ( 'NONE', #14816, #3149, #2190 ) ;
#13885 = CARTESIAN_POINT ( 'NONE',  ( 0.000000000000000000, -96.08423613455721579, 10.65431531532568599 ) ) ;
#13886 = ORIENTED_EDGE ( 'NONE', *, *, #17502, .T. ) ;
#13887 = ADVANCED_FACE ( 'NONE', ( #11618 ), #8999, .T. ) ;
#13888 = ORIENTED_EDGE ( 'NONE', *, *, #9328, .T. ) ;
#13889 = AXIS2_PLACEMENT_3D ( 'NONE', #8757, #788, #7703 ) ;
#13890 = DIRECTION ( 'NONE',  ( 1.156482317317869999E-16, 0.000000000000000000, 1.000000000000000000 ) ) ;
#13891 = DIRECTION ( 'NONE',  ( -0.000000000000000000, -0.000000000000000000, -1.000000000000000000 ) ) ;
#13892 = DIRECTION ( 'NONE',  ( 0.000000000000000000, 0.000000000000000000, -1.000000000000000000 ) ) ;
#13893 = TOROIDAL_SURFACE ( 'NONE', #7323, 47.49926016644946003, 5.000000000000000000 ) ;
#13894 = VERTEX_POINT ( 'NONE', #16009 ) ;
#13895 =( NAMED_UNIT ( * ) SI_UNIT ( $, .STERADIAN. ) SOLID_ANGLE_UNIT ( ) );
#13896 = AXIS2_PLACEMENT_3D ( 'NONE', #1874, #17855, #8988 ) ;
#13897 = CIRCLE ( 'NONE', #3416, 12.50000000000000355 ) ;
#13898 = CARTESIAN_POINT ( 'NONE',  ( 13.61986053733008184, -2.650911626341202254, -51.30709107799135182 ) ) ;
#13899 = CARTESIAN_POINT ( 'NONE',  ( -71.24615306438080609, 110.5319655545637403, 15.00000000000006928 ) ) ;
#13900 = VERTEX_POINT ( 'NONE', #6162 ) ;
#13901 = DIRECTION ( 'NONE',  ( 1.000000000000000000, 0.000000000000000000, 0.000000000000000000 ) ) ;
#13902 = DIRECTION ( 'NONE',  ( 1.000000000000000000, 0.000000000000000000, 0.000000000000000000 ) ) ;
#13903 = DIRECTION ( 'NONE',  ( 2.062304371594500494E-16, -1.000000000000000000, 0.000000000000000000 ) ) ;
#13904 = ORIENTED_EDGE ( 'NONE', *, *, #9492, .F. ) ;
#13905 = CARTESIAN_POINT ( 'NONE',  ( -75.94242511790328365, 106.7395705226562654, -25.18349236146325865 ) ) ;
#13906 = CARTESIAN_POINT ( 'NONE',  ( -102.5926225674731569, 65.58224449241410525, 20.00000000000000355 ) ) ;
#13907 = ORIENTED_EDGE ( 'NONE', *, *, #18104, .F. ) ;
#13908 = DIRECTION ( 'NONE',  ( 0.000000000000000000, -5.551115123125748189E-17, -1.000000000000000000 ) ) ;
#13909 = AXIS2_PLACEMENT_3D ( 'NONE', #15919, #3109, #14521 ) ;
#13910 = LINE ( 'NONE', #8384, #7304 ) ;
#13911 = VECTOR ( 'NONE', #7380, 1000.000000000000000 ) ;
#13912 = ORIENTED_EDGE ( 'NONE', *, *, #12894, .F. ) ;
#13913 = ORIENTED_EDGE ( 'NONE', *, *, #1563, .T. ) ;
#13914 = CARTESIAN_POINT ( 'NONE',  ( -60.71187100093244737, 74.64462966772953223, -167.1454815528550739 ) ) ;
#13915 = CARTESIAN_POINT ( 'NONE',  ( -59.37303238940180705, 94.21775734381046163, -15.00000000000001421 ) ) ;
#13916 = ORIENTED_EDGE ( 'NONE', *, *, #11910, .T. ) ;
#13917 = LINE ( 'NONE', #9505, #1781 ) ;
#13918 = DIRECTION ( 'NONE',  ( 1.000000000000000000, 0.000000000000000000, 0.000000000000000000 ) ) ;
#13919 = CARTESIAN_POINT ( 'NONE',  ( -71.24615306438097662, 57.12489050456376560, -167.1454815528550739 ) ) ;
#13920 = CARTESIAN_POINT ( 'NONE',  ( -98.90286936182231159, -96.08423613455721579, -5.654315315325883162 ) ) ;
#13921 = ORIENTED_EDGE ( 'NONE', *, *, #9320, .F. ) ;
#13922 = EDGE_CURVE ( 'NONE', #13177, #16319, #7493, .T. ) ;
#13923 = CARTESIAN_POINT ( 'NONE',  ( -71.24615306438086293, 93.93513156522925556, 15.00000000000006928 ) ) ;
#13924 = VECTOR ( 'NONE', #13271, 1000.000000000000114 ) ;
#13925 = DIRECTION ( 'NONE',  ( -1.000000000000000000, 0.000000000000000000, 0.000000000000000000 ) ) ;
#13926 = DIRECTION ( 'NONE',  ( 0.9396926207859185309, 0.3420201433256406798, 0.000000000000000000 ) ) ;
#13927 = AXIS2_PLACEMENT_3D ( 'NONE', #13545, #629, #11858 ) ;
#13928 = CARTESIAN_POINT ( 'NONE',  ( 5.233202738124671960, -15.17993412113254337, -54.12718235529279553 ) ) ;
#13929 = FACE_OUTER_BOUND ( 'NONE', #3770, .T. ) ;
#13930 = ORIENTED_EDGE ( 'NONE', *, *, #16015, .T. ) ;
#13931 = DIRECTION ( 'NONE',  ( 1.000000000000000000, 0.000000000000000000, 0.000000000000000000 ) ) ;
#13932 = DIRECTION ( 'NONE',  ( -0.000000000000000000, -0.000000000000000000, -1.000000000000000000 ) ) ;
#13933 = DIRECTION ( 'NONE',  ( -1.000000000000000000, -0.000000000000000000, -0.000000000000000000 ) ) ;
#13934 = DIRECTION ( 'NONE',  ( -0.9475106458593564041, -0.3197242186372270534, 0.000000000000000000 ) ) ;
#13935 = ORIENTED_EDGE ( 'NONE', *, *, #2048, .T. ) ;
#13936 = ORIENTED_EDGE ( 'NONE', *, *, #11252, .T. ) ;
#13937 = DIRECTION ( 'NONE',  ( -1.000000000000000000, 3.016910393003147592E-15, 0.000000000000000000 ) ) ;
#13938 = CYLINDRICAL_SURFACE ( 'NONE', #9418, 4.599999999999999645 ) ;
#13939 = CARTESIAN_POINT ( 'NONE',  ( -107.5926225674731711, 61.64996188551983636, -25.00000000000000000 ) ) ;
#13940 = LINE ( 'NONE', #8128, #10263 ) ;
#13941 = VERTEX_POINT ( 'NONE', #13210 ) ;
#13942 = ADVANCED_FACE ( 'NONE', ( #7766 ), #10582, .T. ) ;
#13943 = LINE ( 'NONE', #18439, #11955 ) ;
#13944 = CARTESIAN_POINT ( 'NONE',  ( 4.699999999999995737, 6.499999999999901412, 2.428612866367529932E-14 ) ) ;
#13945 = CARTESIAN_POINT ( 'NONE',  ( -61.98305514952129158, 93.22868410554717400, 15.00000000000006928 ) ) ;
#13946 = ORIENTED_EDGE ( 'NONE', *, *, #13840, .T. ) ;
#13947 = CARTESIAN_POINT ( 'NONE',  ( -52.04298920050707977, 93.78931001713317528, -15.00000000000001421 ) ) ;
#13948 = CARTESIAN_POINT ( 'NONE',  ( -98.90286936182235422, -91.08423613455721579, -2.027180301682503564E-13 ) ) ;
#13949 = ORIENTED_EDGE ( 'NONE', *, *, #4353, .F. ) ;
#13950 = ADVANCED_FACE ( 'NONE', ( #2060 ), #8904, .T. ) ;
#13951 = DIRECTION ( 'NONE',  ( -2.062304371594500494E-16, 1.000000000000000000, -0.000000000000000000 ) ) ;
#13952 = CYLINDRICAL_SURFACE ( 'NONE', #1164, 10.24900000000000055 ) ;
#13953 = VERTEX_POINT ( 'NONE', #660 ) ;
#13954 = ADVANCED_FACE ( 'NONE', ( #6251 ), #13305, .F. ) ;
#13955 = EDGE_LOOP ( 'NONE', ( #5646, #4865, #16091, #9917 ) ) ;
#13956 = ORIENTED_EDGE ( 'NONE', *, *, #8004, .T. ) ;
#13957 = UNCERTAINTY_MEASURE_WITH_UNIT (LENGTH_MEASURE( 1.000000000000000082E-05 ), #368, 'distance_accuracy_value', 'NONE');
#13958 = EDGE_CURVE ( 'NONE', #17713, #15472, #10612, .T. ) ;
#13959 = CARTESIAN_POINT ( 'NONE',  ( -57.08002265617300708, 84.22855780814606419, 35.00000000000000000 ) ) ;
#13960 = DIRECTION ( 'NONE',  ( -1.000000000000000000, -0.000000000000000000, -0.000000000000000000 ) ) ;
#13961 = EDGE_CURVE ( 'NONE', #2933, #4021, #6078, .T. ) ;
#13962 = DIRECTION ( 'NONE',  ( 0.000000000000000000, 1.000000000000000000, 0.000000000000000000 ) ) ;
#13963 = FACE_OUTER_BOUND ( 'NONE', #5906, .T. ) ;
#13964 = ADVANCED_FACE ( 'NONE', ( #10479 ), #13478, .T. ) ;
#13965 = LINE ( 'NONE', #1145, #5057 ) ;
#13966 = DIRECTION ( 'NONE',  ( 0.000000000000000000, 0.000000000000000000, -1.000000000000000000 ) ) ;
#13967 = ORIENTED_EDGE ( 'NONE', *, *, #5945, .T. ) ;
#13968 = CARTESIAN_POINT ( 'NONE',  ( -68.99615306438067819, 146.5232735881302801, -15.00000000000001421 ) ) ;
#13969 = FACE_OUTER_BOUND ( 'NONE', #16933, .T. ) ;
#13971 = ORIENTED_EDGE ( 'NONE', *, *, #14155, .T. ) ;
#13970 = CARTESIAN_POINT ( 'NONE',  ( -77.62411267699025075, 88.80498052294456102, 68.46181714501862814 ) ) ;
#13972 = CARTESIAN_POINT ( 'NONE',  ( -63.34052343625892689, 73.40930968350525632, 15.00000000000006928 ) ) ;
#13973 = DIRECTION ( 'NONE',  ( 0.000000000000000000, 1.000000000000000000, 0.000000000000000000 ) ) ;
#13974 = ORIENTED_EDGE ( 'NONE', *, *, #10577, .T. ) ;
#13975 = B_SPLINE_CURVE_WITH_KNOTS ( 'NONE', 3,
 ( #10911, #13525, #3789, #2199, #16601, #3700, #608, #7633, #16315, #6486, #17725, #9491 ),
 .UNSPECIFIED., .F., .F.,
 ( 4, 2, 2, 2, 2, 4 ),
 ( 0.009411782824043968959, 0.009923328437046213812, 0.01043487405004845693, 0.01145796527605294490, 0.01248105650205743287, 0.01350414772806192085 ),
 .UNSPECIFIED. ) ;
#13976 = ADVANCED_FACE ( 'NONE', ( #14784 ), #4500, .F. ) ;
#13977 = EDGE_CURVE ( 'NONE', #1187, #14698, #2560, .T. ) ;
#13978 = EDGE_CURVE ( 'NONE', #6648, #4422, #289, .T. ) ;
#13979 = CARTESIAN_POINT ( 'NONE',  ( -71.24615306438070661, 141.9478920545637664, -15.00000000000001421 ) ) ;
#13980 = VERTEX_POINT ( 'NONE', #3275 ) ;
#13981 = EDGE_CURVE ( 'NONE', #3710, #1115, #14783, .T. ) ;
#13982 = VERTEX_POINT ( 'NONE', #11977 ) ;
#13983 = EDGE_CURVE ( 'NONE', #1662, #16693, #5983, .T. ) ;
#13984 = CARTESIAN_POINT ( 'NONE',  ( -71.24615306438076345, 123.0983361545637109, 15.00000000000006928 ) ) ;
#13985 = CARTESIAN_POINT ( 'NONE',  ( -80.43148536604020649, 78.95224028009165806, 92.50000000000000000 ) ) ;
#13986 = ORIENTED_EDGE ( 'NONE', *, *, #6220, .T. ) ;
#13987 = APPLICATION_PROTOCOL_DEFINITION ( 'draft international standard', 'automotive_design', 1998, #3703 ) ;
#13988 = ORIENTED_EDGE ( 'NONE', *, *, #14225, .F. ) ;
#13989 = EDGE_CURVE ( 'NONE', #10224, #12513, #9119, .T. ) ;
#13990 = CARTESIAN_POINT ( 'NONE',  ( 12.67459307379139233, 1.374362345496204174, -50.18803144527930016 ) ) ;
#13991 = ADVANCED_FACE ( 'NONE', ( #8243 ), #16362, .T. ) ;
#13992 = DIRECTION ( 'NONE',  ( 1.000000000000000000, 0.000000000000000000, 0.000000000000000000 ) ) ;
#13993 = ORIENTED_EDGE ( 'NONE', *, *, #4922, .T. ) ;
#13994 = CARTESIAN_POINT ( 'NONE',  ( -46.27380910617147691, 84.15481808402802244, 15.00000000000009592 ) ) ;
#13995 = CARTESIAN_POINT ( 'NONE',  ( -68.43470539589056045, 111.3286264100576801, 22.41764221539786917 ) ) ;
#13996 = DIRECTION ( 'NONE',  ( -1.000000000000000000, 0.000000000000000000, 0.000000000000000000 ) ) ;
#13997 = ORIENTED_EDGE ( 'NONE', *, *, #7443, .F. ) ;
#13998 = CARTESIAN_POINT ( 'NONE',  ( -57.08002265617300708, 84.22855780814606419, 25.00000000000000355 ) ) ;
#13999 = DIRECTION ( 'NONE',  ( 0.000000000000000000, 0.000000000000000000, 1.000000000000000000 ) ) ;
#14000 = ORIENTED_EDGE ( 'NONE', *, *, #14103, .T. ) ;
#14001 = DIRECTION ( 'NONE',  ( -5.204170427930409450E-16, 0.000000000000000000, 1.000000000000000000 ) ) ;
#14002 = DIRECTION ( 'NONE',  ( 1.000000000000000000, 2.062304371594500494E-16, -0.000000000000000000 ) ) ;
#14003 = ORIENTED_EDGE ( 'NONE', *, *, #16977, .F. ) ;
#14004 = CIRCLE ( 'NONE', #11321, 7.168074330099291736 ) ;
#14005 = ORIENTED_EDGE ( 'NONE', *, *, #7113, .F. ) ;
#14006 = LINE ( 'NONE', #12426, #9988 ) ;
#14007 = ORIENTED_EDGE ( 'NONE', *, *, #13483, .T. ) ;
#14008 = LINE ( 'NONE', #5384, #18515 ) ;
#14009 = CARTESIAN_POINT ( 'NONE',  ( 0.000000000000000000, 4.351979364426085531E-16, -6.500000000000039968 ) ) ;
#14010 = CARTESIAN_POINT ( 'NONE',  ( -68.99615306438080609, 105.0677132816627051, -167.1454815528550739 ) ) ;
#14011 = DIRECTION ( 'NONE',  ( -1.000000000000000000, 0.000000000000000000, 0.000000000000000000 ) ) ;
#14012 = VERTEX_POINT ( 'NONE', #17956 ) ;
#14013 = DIRECTION ( 'NONE',  ( -0.9396926207859084279, 0.3420201433256686574, 1.086737899652989892E-16 ) ) ;
#14014 = CYLINDRICAL_SURFACE ( 'NONE', #3452, 4.599999999999999645 ) ;
#14015 = CYLINDRICAL_SURFACE ( 'NONE', #14753, 10.24900000000000766 ) ;
#14016 = CONICAL_SURFACE ( 'NONE', #5642, 6.500000000000039968, 1.047197551196600296 ) ;
#14017 = CARTESIAN_POINT ( 'NONE',  ( -16.92216393104348171, 32.58739983099662396, -37.66730993204898681 ) ) ;
#14018 = CARTESIAN_POINT ( 'NONE',  ( 13.61981611287037808, -2.650921210901910463, 51.30707055644251824 ) ) ;
#14019 = ORIENTED_EDGE ( 'NONE', *, *, #2755, .F. ) ;
#14020 = CARTESIAN_POINT ( 'NONE',  ( -71.24615306438086293, 88.54081700456373483, -15.00000000000001421 ) ) ;
#14021 = CARTESIAN_POINT ( 'NONE',  ( -92.59262256747321373, 117.8748711238780373, -15.00000000000000711 ) ) ;
#14022 = DIRECTION ( 'NONE',  ( -0.000000000000000000, -0.000000000000000000, -1.000000000000000000 ) ) ;
#14023 = CARTESIAN_POINT ( 'NONE',  ( -54.75080917176597950, 94.79374675277695417, -167.1454815528550739 ) ) ;
#14024 = ORIENTED_EDGE ( 'NONE', *, *, #3091, .F. ) ;
#14025 = PRODUCT_RELATED_PRODUCT_CATEGORY ( 'part', '', ( #2679 ) ) ;
#14026 = EDGE_LOOP ( 'NONE', ( #9597, #8766, #1082, #14500 ) ) ;
#14027 = EDGE_CURVE ( 'NONE', #15074, #14163, #867, .T. ) ;
#14028 = VECTOR ( 'NONE', #16696, 1000.000000000000000 ) ;
#14029 = CARTESIAN_POINT ( 'NONE',  ( -107.5926225674731853, 110.5691553257988460, 30.38417033480641294 ) ) ;
#14030 = EDGE_CURVE ( 'NONE', #7906, #10991, #15246, .T. ) ;
#14031 = ORIENTED_EDGE ( 'NONE', *, *, #15334, .F. ) ;
#14032 = CARTESIAN_POINT ( 'NONE',  ( -71.24615306438114715, 12.25372266522925457, -15.00000000000001421 ) ) ;
#14033 = CARTESIAN_POINT ( 'NONE',  ( -50.99714023269321217, 75.97988867778809663, 15.00000000000006928 ) ) ;
#14034 = DIRECTION ( 'NONE',  ( -5.204170427930409450E-16, 0.000000000000000000, 1.000000000000000000 ) ) ;
#14035 = ORIENTED_EDGE ( 'NONE', *, *, #2539, .F. ) ;
#14036 = DIRECTION ( 'NONE',  ( -0.000000000000000000, -0.000000000000000000, 1.000000000000000000 ) ) ;
#14037 = CARTESIAN_POINT ( 'NONE',  ( -71.24615306438080609, 115.9262801152292042, 15.00000000000006928 ) ) ;
#14038 = DIRECTION ( 'NONE',  ( 0.000000000000000000, 1.000000000000000000, 0.000000000000000000 ) ) ;
#14039 = ORIENTED_EDGE ( 'NONE', *, *, #7355, .F. ) ;
#14040 = CARTESIAN_POINT ( 'NONE',  ( -71.24615306438096241, 63.40807580456375803, -15.00000000000001421 ) ) ;
#14041 = AXIS2_PLACEMENT_3D ( 'NONE', #14186, #1373, #14540 ) ;
#14042 = ORIENTED_EDGE ( 'NONE', *, *, #6841, .T. ) ;
#14043 = DIRECTION ( 'NONE',  ( -1.000000000000000000, -0.000000000000000000, -0.000000000000000000 ) ) ;
#14044 = CIRCLE ( 'NONE', #4461, 4.599999999999992539 ) ;
#14045 = DIRECTION ( 'NONE',  ( 1.000000000000000000, 0.000000000000000000, -0.000000000000000000 ) ) ;
#14046 = ORIENTED_EDGE ( 'NONE', *, *, #9629, .T. ) ;
#14047 = ORIENTED_EDGE ( 'NONE', *, *, #16248, .F. ) ;
#14048 = VERTEX_POINT ( 'NONE', #3834 ) ;
#14049 = DIRECTION ( 'NONE',  ( -0.000000000000000000, 1.000000000000000000, -0.000000000000000000 ) ) ;
#14050 = CARTESIAN_POINT ( 'NONE',  ( -71.24615306438113294, 13.14259340456378489, -15.00000000000001421 ) ) ;
#14051 = VECTOR ( 'NONE', #3273, 1000.000000000000000 ) ;
#14052 = CARTESIAN_POINT ( 'NONE',  ( -92.59262256747319952, 60.58224449241411946, 35.00000000000000000 ) ) ;
#14053 = DIRECTION ( 'NONE',  ( -0.000000000000000000, -0.000000000000000000, -1.000000000000000000 ) ) ;
#14054 = EDGE_CURVE ( 'NONE', #16133, #288, #5326, .T. ) ;
#14055 = DIRECTION ( 'NONE',  ( 0.000000000000000000, 0.000000000000000000, 1.000000000000000000 ) ) ;
#14056 = VECTOR ( 'NONE', #17014, 1000.000000000000000 ) ;
#14057 = CARTESIAN_POINT ( 'NONE',  ( 0.4037800551814025307, 4.058962678540093627, -5.969670414742754616 ) ) ;
#14058 = VERTEX_POINT ( 'NONE', #15350 ) ;
#14059 = LINE ( 'NONE', #207, #7226 ) ;
#14060 = ORIENTED_EDGE ( 'NONE', *, *, #5956, .T. ) ;
#14061 = CARTESIAN_POINT ( 'NONE',  ( -107.5926225674731711, 57.88796029049330372, 22.35917033480642502 ) ) ;
#14062 = CARTESIAN_POINT ( 'NONE',  ( -65.18918009136295666, 110.5691553257988318, 26.35917033480641436 ) ) ;
#14063 = ORIENTED_EDGE ( 'NONE', *, *, #678, .T. ) ;
#14064 = FACE_OUTER_BOUND ( 'NONE', #7943, .T. ) ;
#14065 = ORIENTED_EDGE ( 'NONE', *, *, #10485, .F. ) ;
#14067 = EDGE_CURVE ( 'NONE', #14807, #14603, #7929, .T. ) ;
#14066 = CIRCLE ( 'NONE', #14363, 3.999999999999989786 ) ;
#14068 = EDGE_CURVE ( 'NONE', #4994, #409, #16731, .T. ) ;
#14069 = VECTOR ( 'NONE', #1389, 1000.000000000000000 ) ;
#14070 = VECTOR ( 'NONE', #12551, 1000.000000000000000 ) ;
#14071 = EDGE_LOOP ( 'NONE', ( #10941, #291, #11814, #831 ) ) ;
#14072 = FILL_AREA_STYLE ('',( #8362 ) ) ;
#14073 = LINE ( 'NONE', #8461, #10562 ) ;
#14074 = CARTESIAN_POINT ( 'NONE',  ( -68.99615306438076345, 118.2489397381302751, -15.00000000000001421 ) ) ;
#14075 = EDGE_CURVE ( 'NONE', #12741, #16981, #18059, .T. ) ;
#14076 = VERTEX_POINT ( 'NONE', #12263 ) ;
#14077=STYLED_ITEM('',(#18566),#6235);
#14078 = ADVANCED_FACE ( 'NONE', ( #8039 ), #9642, .T. ) ;
#14079 = ORIENTED_EDGE ( 'NONE', *, *, #4562, .T. ) ;
#14080 = CARTESIAN_POINT ( 'NONE',  ( -68.99615306438072082, 127.0588618316627105, -167.1454815528550739 ) ) ;
#14081 = VECTOR ( 'NONE', #7515, 1000.000000000000000 ) ;
#14082 = DIRECTION ( 'NONE',  ( -6.608470384673552010E-16, 0.000000000000000000, -1.000000000000000000 ) ) ;
#14083 = ORIENTED_EDGE ( 'NONE', *, *, #11473, .T. ) ;
#14084 = CARTESIAN_POINT ( 'NONE',  ( -57.08002265617300708, 84.22855780814606419, -167.1454815528550739 ) ) ;
#14085 = PLANE ( 'NONE',  #1866 ) ;
#14086 = VECTOR ( 'NONE', #4631, 1000.000000000000000 ) ;
#14087 = ORIENTED_EDGE ( 'NONE', *, *, #16106, .F. ) ;
#14088 = DIRECTION ( 'NONE',  ( -1.000000000000000000, 0.000000000000000000, -0.000000000000000000 ) ) ;
#14089 = DIRECTION ( 'NONE',  ( -1.000000000000000000, -0.000000000000000000, 1.156482317317869999E-16 ) ) ;
#14090 = EDGE_LOOP ( 'NONE', ( #17787, #7435, #15392, #11729, #5406 ) ) ;
#14091 = EDGE_CURVE ( 'NONE', #7683, #4700, #6743, .T. ) ;
#14092 = CARTESIAN_POINT ( 'NONE',  ( -60.18936887439735273, 72.12145385653096241, -15.00000000000001421 ) ) ;
#14093 = EDGE_CURVE ( 'NONE', #6728, #18478, #5240, .T. ) ;
#14094 = LINE ( 'NONE', #16891, #4316 ) ;
#14095 = ORIENTED_EDGE ( 'NONE', *, *, #9721, .F. ) ;
#14096 = EDGE_CURVE ( 'NONE', #6867, #15862, #17778, .T. ) ;
#14097 = ADVANCED_FACE ( 'NONE', ( #2629 ), #14140, .T. ) ;
#14098 = VECTOR ( 'NONE', #5258, 1000.000000000000000 ) ;
#14099 = AXIS2_PLACEMENT_3D ( 'NONE', #10345, #17258, #7627 ) ;
#14100 = LINE ( 'NONE', #10067, #7007 ) ;
#14101 = DIRECTION ( 'NONE',  ( 0.000000000000000000, 0.000000000000000000, -1.000000000000000000 ) ) ;
#14102 = CARTESIAN_POINT ( 'NONE',  ( 5.299999999999998934, 0.000000000000000000, 0.000000000000000000 ) ) ;
#14103 = EDGE_CURVE ( 'NONE', #8931, #13353, #4216, .T. ) ;
#14104 = ORIENTED_EDGE ( 'NONE', *, *, #12482, .F. ) ;
#14105 = LINE ( 'NONE', #15495, #11047 ) ;
#14106 = DIRECTION ( 'NONE',  ( -1.000000000000000000, 5.416250486023796615E-15, 1.692578276882436442E-16 ) ) ;
#14107 = DIRECTION ( 'NONE',  ( 0.000000000000000000, 0.000000000000000000, 1.000000000000000000 ) ) ;
#14108 = CARTESIAN_POINT ( 'NONE',  ( -49.58002265617300708, 84.22855780814606419, 15.00000000000007283 ) ) ;
#14109 = ORIENTED_EDGE ( 'NONE', *, *, #6957, .F. ) ;
#14110 = CIRCLE ( 'NONE', #14972, 12.29357405616490695 ) ;
#14111 = DIRECTION ( 'NONE',  ( -1.000000000000000000, 3.016910393003138520E-15, 0.000000000000000000 ) ) ;
#14112 = PLANE ( 'NONE',  #141 ) ;
#14113 = CARTESIAN_POINT ( 'NONE',  ( -15.52181756281650493, 31.21008990100222391, -38.37361753973598155 ) ) ;
#14114 = CARTESIAN_POINT ( 'NONE',  ( 12.67495189244583287, 1.372358515719736882, 50.18853589267851589 ) ) ;
#14115 = ORIENTED_EDGE ( 'NONE', *, *, #907, .T. ) ;
#14116 = CIRCLE ( 'NONE', #10213, 5.654315315325682434 ) ;
#14117 = AXIS2_PLACEMENT_3D ( 'NONE', #16076, #8989, #1875 ) ;
#14118 = CARTESIAN_POINT ( 'NONE',  ( -64.09025127992791226, 109.3109350805793270, 35.00000000000000000 ) ) ;
#14119 = CARTESIAN_POINT ( 'NONE',  ( -68.99615306438100504, 49.13390143813029454, -167.1454815528550739 ) ) ;
#14120 = CARTESIAN_POINT ( 'NONE',  ( -92.59262256747319952, 57.88796029049329661, -26.35917033480641436 ) ) ;
#14121 = LINE ( 'NONE', #1310, #13762 ) ;
#14122 = ORIENTED_EDGE ( 'NONE', *, *, #6530, .F. ) ;
#14123 = VERTEX_POINT ( 'NONE', #4040 ) ;
#14124 = AXIS2_PLACEMENT_3D ( 'NONE', #16909, #15215, #11021 ) ;
#14125 = CARTESIAN_POINT ( 'NONE',  ( 0.4037800551814653138, -7.199367570657762450, -0.5303295852573244318 ) ) ;
#14126 = VECTOR ( 'NONE', #13547, 1000.000000000000000 ) ;
#14127 = AXIS2_PLACEMENT_3D ( 'NONE', #7116, #9486, #16059 ) ;
#14128 = LINE ( 'NONE', #15517, #12730 ) ;
#14129 = DIRECTION ( 'NONE',  ( 1.000000000000000000, 0.000000000000000000, -0.000000000000000000 ) ) ;
#14130 = CARTESIAN_POINT ( 'NONE',  ( -65.06546592763082515, -96.08423613455721579, -45.05044770573174873 ) ) ;
#14131 = EDGE_LOOP ( 'NONE', ( #6773, #16855, #16321, #10803 ) ) ;
#14132 = CARTESIAN_POINT ( 'NONE',  ( -68.99615306438104767, 20.85956758813029310, 15.00000000000006928 ) ) ;
#14133 = CARTESIAN_POINT ( 'NONE',  ( -57.08002265617300708, 84.22855780814606419, 15.00000000000006928 ) ) ;
#14134 = CARTESIAN_POINT ( 'NONE',  ( 0.000000000000000000, -4.857225732735059864E-14, 6.500000000000037303 ) ) ;
#14135 = ORIENTED_EDGE ( 'NONE', *, *, #5959, .F. ) ;
#14136 = AXIS2_PLACEMENT_3D ( 'NONE', #17890, #5073, #3686 ) ;
#14137 = CARTESIAN_POINT ( 'NONE',  ( -69.37109144396066540, 81.95267818613797317, -167.1454815528550739 ) ) ;
#14138 = ORIENTED_EDGE ( 'NONE', *, *, #14604, .T. ) ;
#14139 = CIRCLE ( 'NONE', #11736, 12.50000000000000355 ) ;
#14140 = CYLINDRICAL_SURFACE ( 'NONE', #4765, 4.599999999999999645 ) ;
#14141 = AXIS2_PLACEMENT_3D ( 'NONE', #11905, #7509, #5837 ) ;
#14142 = CARTESIAN_POINT ( 'NONE',  ( -57.08002265617300708, 84.22855780814606419, 15.00000000000006573 ) ) ;
#14143 = ORIENTED_EDGE ( 'NONE', *, *, #13405, .T. ) ;
#14144 = ORIENTED_EDGE ( 'NONE', *, *, #4636, .T. ) ;
#14145 = ORIENTED_EDGE ( 'NONE', *, *, #14312, .T. ) ;
#14146 = VECTOR ( 'NONE', #11512, 1000.000000000000000 ) ;
#14147 = DIRECTION ( 'NONE',  ( 0.3420201433256686574, -0.9396926207859084279, 0.000000000000000000 ) ) ;
#14148 = CARTESIAN_POINT ( 'NONE',  ( -71.24615306438083451, 97.07672421522921979, -167.1454815528550739 ) ) ;
#14149 = DIRECTION ( 'NONE',  ( -0.000000000000000000, -1.000000000000000000, 0.000000000000000000 ) ) ;
#14150 = VECTOR ( 'NONE', #17219, 1000.000000000000114 ) ;
#14151 = DIRECTION ( 'NONE',  ( 0.000000000000000000, 0.000000000000000000, 1.000000000000000000 ) ) ;
#14152 = VECTOR ( 'NONE', #1246, 1000.000000000000114 ) ;
#14153 = CARTESIAN_POINT ( 'NONE',  ( -71.24615306438086293, 87.65194626522927024, -167.1454815528550739 ) ) ;
#14154 = ORIENTED_EDGE ( 'NONE', *, *, #13163, .T. ) ;
#14155 = EDGE_CURVE ( 'NONE', #15720, #18116, #13, .T. ) ;
#14156 = PLANE ( 'NONE',  #16763 ) ;
#14157 = ORIENTED_EDGE ( 'NONE', *, *, #7306, .T. ) ;
#14158 = CARTESIAN_POINT ( 'NONE',  ( -198.5768363665157494, 84.22855780814606419, 62.50000000000001421 ) ) ;
#14159 = DIRECTION ( 'NONE',  ( -1.000000000000000000, 0.000000000000000000, 0.000000000000000000 ) ) ;
#14160 = VERTEX_POINT ( 'NONE', #9745 ) ;
#14161 = AXIS2_PLACEMENT_3D ( 'NONE', #10678, #9460, #15154 ) ;
#14162 = LINE ( 'NONE', #1698, #16659 ) ;
#14163 = VERTEX_POINT ( 'NONE', #5530 ) ;
#14164 = ADVANCED_FACE ( 'NONE', ( #15636 ), #14321, .T. ) ;
#14165 = PRODUCT_DEFINITION_FORMATION_WITH_SPECIFIED_SOURCE ( 'ANY', '', #10574, .NOT_KNOWN. ) ;
#14166 = AXIS2_PLACEMENT_3D ( 'NONE', #5200, #9321, #10638 ) ;
#14167 = VECTOR ( 'NONE', #15474, 1000.000000000000000 ) ;
#14168 = VERTEX_POINT ( 'NONE', #18249 ) ;
#14169 = CARTESIAN_POINT ( 'NONE',  ( -65.06546592763099568, -96.08423613455721579, -28.18308811886532084 ) ) ;
#14170 = CARTESIAN_POINT ( 'NONE',  ( -67.59262256747319952, 110.5691553257988460, 22.35917033480642502 ) ) ;
#14171 = ADVANCED_BREP_SHAPE_REPRESENTATION ( '', ( #6235, #16217 ), #3695 ) ;
#14172 = VECTOR ( 'NONE', #8388, 1000.000000000000000 ) ;
#14173 = VERTEX_POINT ( 'NONE', #11253 ) ;
#14174 = ITEM_DEFINED_TRANSFORMATION ( 'NONE', 'NONE', #7567,  #16217 ) ;
#14175 = VERTEX_POINT ( 'NONE', #8705 ) ;
#14176 = CARTESIAN_POINT ( 'NONE',  ( -9.438806153496912543, 39.35910582506906508, -33.99713577918199547 ) ) ;
#14177 = DIRECTION ( 'NONE',  ( 0.000000000000000000, 0.000000000000000000, 1.000000000000000000 ) ) ;
#14178 = ORIENTED_EDGE ( 'NONE', *, *, #5942, .T. ) ;
#14179 = DIRECTION ( 'NONE',  ( -0.000000000000000000, -0.000000000000000000, -1.000000000000000000 ) ) ;
#14180 = DIRECTION ( 'NONE',  ( 1.000000000000000000, 0.000000000000000000, 0.000000000000000000 ) ) ;
#14181 = EDGE_CURVE ( 'NONE', #11028, #1745, #2994, .T. ) ;
#14182 = CARTESIAN_POINT ( 'NONE',  ( 44.74549999999999272, 2.678141147339113553E-16, -4.000000000000000000 ) ) ;
#14183 = AXIS2_PLACEMENT_3D ( 'NONE', #14570, #17463, #12046 ) ;
#14184 = VERTEX_POINT ( 'NONE', #10025 ) ;
#14185 = VECTOR ( 'NONE', #13313, 1000.000000000000000 ) ;
#14186 = CARTESIAN_POINT ( 'NONE',  ( -68.99615306438072082, 130.2004544816626890, -167.1454815528550739 ) ) ;
#14187 = ORIENTED_EDGE ( 'NONE', *, *, #14634, .T. ) ;
#14188 = CARTESIAN_POINT ( 'NONE',  ( -123.4618227840623632, -151.5628872026273086, 57.00000000000000000 ) ) ;
#14189 = EDGE_LOOP ( 'NONE', ( #13157, #4982, #7106, #13318 ) ) ;
#14190 = ADVANCED_FACE ( 'NONE', ( #8328 ), #8431, .T. ) ;
#14191 = CARTESIAN_POINT ( 'NONE',  ( -68.99615306438086293, 89.97460588813027016, 15.00000000000006928 ) ) ;
#14192 = VERTEX_POINT ( 'NONE', #1500 ) ;
#14193 = VECTOR ( 'NONE', #16255, 1000.000000000000000 ) ;
#14194 = ADVANCED_FACE ( 'NONE', ( #1904 ), #15531, .T. ) ;
#14195 = VECTOR ( 'NONE', #10154, 999.9999999999998863 ) ;
#14196 = VECTOR ( 'NONE', #18433, 1000.000000000000000 ) ;
#14197 = VERTEX_POINT ( 'NONE', #5423 ) ;
#14198 = DIRECTION ( 'NONE',  ( -0.9913829028484120176, 0.1309959539064320944, 0.000000000000000000 ) ) ;
#14199 = FACE_OUTER_BOUND ( 'NONE', #6031, .T. ) ;
#14200 = EDGE_LOOP ( 'NONE', ( #2632, #16524, #10912, #4329, #7798, #543, #1259, #17358 ) ) ;
#14201 = EDGE_CURVE ( 'NONE', #18427, #12358, #12657, .T. ) ;
#14202 = CARTESIAN_POINT ( 'NONE',  ( -127.5926225674731711, 61.53592931583062864, -28.00000000000000355 ) ) ;
#14203 = CARTESIAN_POINT ( 'NONE',  ( -83.12361985383350316, 84.22855780814606419, 37.50000000000000000 ) ) ;
#14204 = DIRECTION ( 'NONE',  ( 0.000000000000000000, 0.000000000000000000, -1.000000000000000000 ) ) ;
#14205 = EDGE_CURVE ( 'NONE', #14448, #18509, #17334, .T. ) ;
#14206 = LINE ( 'NONE', #5668, #13000 ) ;
#14207 = ORIENTED_EDGE ( 'NONE', *, *, #4242, .F. ) ;
#14208 = EDGE_CURVE ( 'NONE', #6726, #2809, #16842, .T. ) ;
#14209 = LINE ( 'NONE', #8101, #5975 ) ;
#14210 = ADVANCED_FACE ( 'NONE', ( #7039 ), #13169, .T. ) ;
#14211 = CARTESIAN_POINT ( 'NONE',  ( 3.839657907260265013, -5.121192436768893685, -51.90027309438220016 ) ) ;
#14212 = PLANE ( 'NONE',  #6025 ) ;
#14213 = ORIENTED_EDGE ( 'NONE', *, *, #14956, .F. ) ;
#14214 = CIRCLE ( 'NONE', #4330, 3.999999999999989786 ) ;
#14215 = AXIS2_PLACEMENT_3D ( 'NONE', #14133, #7379, #5691 ) ;
#14216 = LINE ( 'NONE', #10000, #13287 ) ;
#14217 = CARTESIAN_POINT ( 'NONE',  ( -68.99615306438083451, 98.78452798166264870, -15.00000000000001421 ) ) ;
#14218 = EDGE_CURVE ( 'NONE', #6290, #5248, #1228, .T. ) ;
#14219 = ADVANCED_FACE ( 'NONE', ( #5613 ), #9928, .T. ) ;
#14220 = DIRECTION ( 'NONE',  ( -1.000000000000000000, 0.000000000000000000, 0.000000000000000000 ) ) ;
#14221 = EDGE_CURVE ( 'NONE', #797, #11906, #1418, .T. ) ;
#14222 = CARTESIAN_POINT ( 'NONE',  ( -73.32517902883354566, 66.64375664990241432, 97.49999999999998579 ) ) ;
#14223 = EDGE_LOOP ( 'NONE', ( #589, #5362, #4407, #9523 ) ) ;
#14224 = ORIENTED_EDGE ( 'NONE', *, *, #17491, .T. ) ;
#14225 = EDGE_CURVE ( 'NONE', #2768, #17254, #10919, .T. ) ;
#14226 = DIRECTION ( 'NONE',  ( 0.3420201433256444545, -0.9396926207859171987, 0.000000000000000000 ) ) ;
#14227 = VERTEX_POINT ( 'NONE', #3083 ) ;
#14228 = AXIS2_PLACEMENT_3D ( 'NONE', #2218, #5013, #10726 ) ;
#14229 = CARTESIAN_POINT ( 'NONE',  ( -71.24615306438097662, 62.51920506522922949, -167.1454815528550739 ) ) ;
#14230 = CARTESIAN_POINT ( 'NONE',  ( -68.99615306438089135, 83.07656473166271383, 15.00000000000006928 ) ) ;
#14231 = CARTESIAN_POINT ( 'NONE',  ( -127.5926225674732279, 47.87487112387803023, 15.00000000000004263 ) ) ;
#14232 = ORIENTED_EDGE ( 'NONE', *, *, #5172, .F. ) ;
#14233 = CARTESIAN_POINT ( 'NONE',  ( -57.08002265617300708, 84.22855780814606419, -61.50000000000001421 ) ) ;
#14234 = CYLINDRICAL_SURFACE ( 'NONE', #4638, 45.40389983439752086 ) ;
#14235 = EDGE_CURVE ( 'NONE', #13480, #16207, #11690, .T. ) ;
#14236 = SURFACE_STYLE_FILL_AREA ( #17145 ) ;
#14237 = CYLINDRICAL_SURFACE ( 'NONE', #968, 10.24899999999999345 ) ;
#14238 = ORIENTED_EDGE ( 'NONE', *, *, #1933, .T. ) ;
#14239 = ADVANCED_FACE ( 'NONE', ( #14580 ), #16156, .T. ) ;
#14240 = DIRECTION ( 'NONE',  ( 0.3420201433256649937, -0.9396926207859097602, 0.000000000000000000 ) ) ;
#14241 = ORIENTED_EDGE ( 'NONE', *, *, #12838, .F. ) ;
#14242 = DIRECTION ( 'NONE',  ( 0.000000000000000000, 0.000000000000000000, -1.000000000000000000 ) ) ;
#14243 = SURFACE_STYLE_FILL_AREA ( #8536 ) ;
#14244 = EDGE_LOOP ( 'NONE', ( #15886, #8146, #17973, #2772 ) ) ;
#14245 = ORIENTED_EDGE ( 'NONE', *, *, #344, .F. ) ;
#14246 = ORIENTED_EDGE ( 'NONE', *, *, #4795, .T. ) ;
#14247 = LINE ( 'NONE', #16948, #16866 ) ;
#14248 = LINE ( 'NONE', #9935, #2805 ) ;
#14249 = CARTESIAN_POINT ( 'NONE',  ( -78.05508519719376181, 82.51445519007735641, 69.80563559789565886 ) ) ;
#14250 = CARTESIAN_POINT ( 'NONE',  ( -45.85876501399108207, 78.72098330317804482, -15.00000000000001421 ) ) ;
#14251 = CARTESIAN_POINT ( 'NONE',  ( 79.02261728059691848, -151.5628872026273086, -57.00000000000000000 ) ) ;
#14252 = ORIENTED_EDGE ( 'NONE', *, *, #2628, .T. ) ;
#14253 = PLANE ( 'NONE',  #1546 ) ;
#14254 = ORIENTED_EDGE ( 'NONE', *, *, #3536, .T. ) ;
#14255 = DIRECTION ( 'NONE',  ( -0.9396926207859097602, 0.3420201433256649937, 1.086737899652991371E-16 ) ) ;
#14256 = PLANE ( 'NONE',  #3576 ) ;
#14257 = ORIENTED_EDGE ( 'NONE', *, *, #459, .F. ) ;
#14258 = SHAPE_REPRESENTATION ( 'High-Ratio Toggle Operating Handle', ( #16217 ), #2194 ) ;
#14259 = FACE_OUTER_BOUND ( 'NONE', #805, .T. ) ;
#14260 = ORIENTED_EDGE ( 'NONE', *, *, #8907, .F. ) ;
#14261 = EDGE_CURVE ( 'NONE', #5721, #6695, #3345, .T. ) ;
#14262 = ORIENTED_EDGE ( 'NONE', *, *, #9951, .T. ) ;
#14263 = LINE ( 'NONE', #6860, #430 ) ;
#14264 = CARTESIAN_POINT ( 'NONE',  ( -71.24615306438090556, 72.83285375456371469, -15.00000000000001421 ) ) ;
#14265 = LINE ( 'NONE', #13126, #13521 ) ;
#14266 = VERTEX_POINT ( 'NONE', #6053 ) ;
#14267 = EDGE_CURVE ( 'NONE', #14163, #6267, #8799, .T. ) ;
#14268 = ORIENTED_EDGE ( 'NONE', *, *, #11765, .F. ) ;
#14269 = CARTESIAN_POINT ( 'NONE',  ( 0.000000000000000000, -2.914335439641035919E-13, -6.500000000000019540 ) ) ;
#14270 = LINE ( 'NONE', #8281, #17175 ) ;
#14271 = ORIENTED_EDGE ( 'NONE', *, *, #18277, .T. ) ;
#14272 = DIRECTION ( 'NONE',  ( 1.000000000000000000, 0.000000000000000000, 3.771137991253928573E-16 ) ) ;
#14273 = FACE_OUTER_BOUND ( 'NONE', #16299, .T. ) ;
#14274 = CARTESIAN_POINT ( 'NONE',  ( -68.99615306438083451, 98.78452798166264870, -167.1454815528550739 ) ) ;
#14275 = VERTEX_POINT ( 'NONE', #3447 ) ;
#14276 = FACE_OUTER_BOUND ( 'NONE', #1594, .T. ) ;
#14277 = ORIENTED_EDGE ( 'NONE', *, *, #11698, .F. ) ;
#14278 = EDGE_LOOP ( 'NONE', ( #12037, #13068, #6849, #16699 ) ) ;
#14279 = CARTESIAN_POINT ( 'NONE',  ( -71.24615306438086293, 91.68240965456375591, 15.00000000000006928 ) ) ;
#14280 = VERTEX_POINT ( 'NONE', #13362 ) ;
#14281 = VERTEX_POINT ( 'NONE', #9070 ) ;
#14282 = VERTEX_POINT ( 'NONE', #8886 ) ;
#14283 = CARTESIAN_POINT ( 'NONE',  ( -127.5926225674731995, 110.5691553257988460, -26.35917033480641436 ) ) ;
#14284 = CARTESIAN_POINT ( 'NONE',  ( -64.09025127992791226, 117.8748711238780373, -35.00000000000000000 ) ) ;
#14285 = ORIENTED_EDGE ( 'NONE', *, *, #11980, .T. ) ;
#14286 = DIRECTION ( 'NONE',  ( 1.000000000000000000, 0.000000000000000000, 0.000000000000000000 ) ) ;
#14287 = CARTESIAN_POINT ( 'NONE',  ( -71.24615306438094819, 69.69126110456375045, -167.1454815528550739 ) ) ;
#14288 = CARTESIAN_POINT ( 'NONE',  ( -71.24615306438070661, 134.7758360152292312, -15.00000000000001421 ) ) ;
#14289 = CARTESIAN_POINT ( 'NONE',  ( -97.59262256747318531, 57.88796029049330372, 22.35917033480642502 ) ) ;
#14290 = EDGE_LOOP ( 'NONE', ( #14024, #78, #5015, #15411 ) ) ;
#14291 = EDGE_CURVE ( 'NONE', #8437, #2855, #5083, .T. ) ;
#14292 = FACE_OUTER_BOUND ( 'NONE', #2608, .T. ) ;
#14293 = CARTESIAN_POINT ( 'NONE',  ( -71.24615306438076345, 132.5231141045637457, -167.1454815528550739 ) ) ;
#14294 = ORIENTED_EDGE ( 'NONE', *, *, #11215, .F. ) ;
#14295 = FACE_OUTER_BOUND ( 'NONE', #14189, .T. ) ;
#14296 = LINE ( 'NONE', #6006, #14081 ) ;
#14297 = CIRCLE ( 'NONE', #6509, 12.50000000000000355 ) ;
#14298 = CARTESIAN_POINT ( 'NONE',  ( -68.99615306438066398, 140.2400882881302664, 15.00000000000006928 ) ) ;
#14299 = CARTESIAN_POINT ( 'NONE',  ( -31.03642545851250745, 84.22855780814606419, 37.50000000000000000 ) ) ;
#14300 = ORIENTED_EDGE ( 'NONE', *, *, #5866, .F. ) ;
#14301 = ADVANCED_FACE ( 'NONE', ( #14501 ), #10170, .F. ) ;
#14302 = VERTEX_POINT ( 'NONE', #8973 ) ;
#14303 = EDGE_CURVE ( 'NONE', #768, #3406, #6259, .T. ) ;
#14304 = ORIENTED_EDGE ( 'NONE', *, *, #3691, .T. ) ;
#14305 = CYLINDRICAL_SURFACE ( 'NONE', #6730, 4.599999999999992539 ) ;
#14306 = CIRCLE ( 'NONE', #6524, 42.49926016644912607 ) ;
#14307 = DIRECTION ( 'NONE',  ( 0.000000000000000000, -5.551115123125747573E-17, -1.000000000000000000 ) ) ;
#14308 = ORIENTED_EDGE ( 'NONE', *, *, #11114, .F. ) ;
#14309 = ADVANCED_FACE ( 'NONE', ( #14762 ), #1589, .T. ) ;
#14310 = ADVANCED_FACE ( 'NONE', ( #17557 ), #195, .T. ) ;
#14311 = DIRECTION ( 'NONE',  ( -5.204170427930409450E-16, 0.000000000000000000, 1.000000000000000000 ) ) ;
#14312 = EDGE_CURVE ( 'NONE', #11918, #11230, #6139, .T. ) ;
#14313 = DIRECTION ( 'NONE',  ( 1.000000000000000000, 0.000000000000000000, 0.000000000000000000 ) ) ;
#14314 = CARTESIAN_POINT ( 'NONE',  ( 113.3630170098443273, -111.0842361345571874, 7.000000000000010658 ) ) ;
#14315 = DIRECTION ( 'NONE',  ( 0.000000000000000000, 0.000000000000000000, 1.000000000000000000 ) ) ;
#14316 = VERTEX_POINT ( 'NONE', #5882 ) ;
#14317 = CARTESIAN_POINT ( 'NONE',  ( -68.99615306438072082, 139.6252324316626812, -15.00000000000001421 ) ) ;
#14318 = PLANE ( 'NONE',  #11964 ) ;
#14319 = VERTEX_POINT ( 'NONE', #11601 ) ;
#14320 = ADVANCED_FACE ( 'NONE', ( #17293 ), #4479, .T. ) ;
#14321 = PLANE ( 'NONE',  #10462 ) ;
#14322 = CARTESIAN_POINT ( 'NONE',  ( -46.03642545851250389, 84.22855780814606419, -124.8487082408420861 ) ) ;
#14323 = ORIENTED_EDGE ( 'NONE', *, *, #16366, .F. ) ;
#14324 = AXIS2_PLACEMENT_3D ( 'NONE', #17129, #14149, #8811 ) ;
#14325 = ORIENTED_EDGE ( 'NONE', *, *, #17276, .T. ) ;
#14326 = ADVANCED_FACE ( 'NONE', ( #6618, #16429 ), #741, .T. ) ;
#14327 = EDGE_CURVE ( 'NONE', #3086, #2130, #13831, .T. ) ;
#14328 = DIRECTION ( 'NONE',  ( 1.000000000000000000, 4.675871521838984962E-16, -0.000000000000000000 ) ) ;
#14329 = CARTESIAN_POINT ( 'NONE',  ( -123.4618227840623632, -151.5628872026273086, 57.00000000000000000 ) ) ;
#14330 = LINE ( 'NONE', #4226, #4740 ) ;
#14331 = EDGE_CURVE ( 'NONE', #11390, #10920, #3281, .T. ) ;
#14332 = LINE ( 'NONE', #4321, #10443 ) ;
#14333 = DIRECTION ( 'NONE',  ( 0.000000000000000000, 0.000000000000000000, 1.000000000000000000 ) ) ;
#14334 = ORIENTED_EDGE ( 'NONE', *, *, #3999, .T. ) ;
#14335 = FACE_OUTER_BOUND ( 'NONE', #3754, .T. ) ;
#14336 = ORIENTED_EDGE ( 'NONE', *, *, #9247, .T. ) ;
#14337 = CARTESIAN_POINT ( 'NONE',  ( -77.34864400865063772, -93.09900722835554632, 43.93281456327058265 ) ) ;
#14338 = VECTOR ( 'NONE', #12132, 1000.000000000000000 ) ;
#14339 = LINE ( 'NONE', #5896, #10456 ) ;
#14340 = ORIENTED_EDGE ( 'NONE', *, *, #18315, .F. ) ;
#14341 = PLANE ( 'NONE',  #15491 ) ;
#14342 = VERTEX_POINT ( 'NONE', #6519 ) ;
#14343 = VECTOR ( 'NONE', #3467, 1000.000000000000000 ) ;
#14344 = ORIENTED_EDGE ( 'NONE', *, *, #14871, .F. ) ;
#14345 = CIRCLE ( 'NONE', #2091, 12.49999999999999112 ) ;
#14346 = CARTESIAN_POINT ( 'NONE',  ( -68.99615306438111872, 10.81993378166265529, 15.00000000000006928 ) ) ;
#14347 = CARTESIAN_POINT ( 'NONE',  ( -68.99615306438067819, 145.9084177316626949, 15.00000000000006928 ) ) ;
#14348 = ORIENTED_EDGE ( 'NONE', *, *, #10190, .T. ) ;
#14349 = ORIENTED_EDGE ( 'NONE', *, *, #12077, .T. ) ;
#14350 = CARTESIAN_POINT ( 'NONE',  ( -71.24615306438106188, 35.13374195456378146, -167.1454815528550739 ) ) ;
#14351 = DIRECTION ( 'NONE',  ( -0.000000000000000000, -0.000000000000000000, -1.000000000000000000 ) ) ;
#14352 = CARTESIAN_POINT ( 'NONE',  ( -57.08002265617300708, 84.22855780814606419, 68.73600986863397111 ) ) ;
#14353 = ORIENTED_EDGE ( 'NONE', *, *, #6866, .T. ) ;
#14354 = CIRCLE ( 'NONE', #15239, 10.24900000000000055 ) ;
#14355 = DIRECTION ( 'NONE',  ( 0.000000000000000000, 1.000000000000000000, -0.000000000000000000 ) ) ;
#14357 = ORIENTED_EDGE ( 'NONE', *, *, #9255, .T. ) ;
#14356 = PRODUCT_RELATED_PRODUCT_CATEGORY ( 'part', '', ( #2051 ) ) ;
#14358 = VECTOR ( 'NONE', #11876, 1000.000000000000114 ) ;
#14359 = VERTEX_POINT ( 'NONE', #7940 ) ;
#14360 = ORIENTED_EDGE ( 'NONE', *, *, #11885, .F. ) ;
#14361 = AXIS2_PLACEMENT_3D ( 'NONE', #5883, #14502, #7387 ) ;
#14362 = ORIENTED_EDGE ( 'NONE', *, *, #972, .F. ) ;
#14363 = AXIS2_PLACEMENT_3D ( 'NONE', #16153, #637, #10556 ) ;
#14364 = DIRECTION ( 'NONE',  ( 0.000000000000000000, 0.000000000000000000, 1.000000000000000000 ) ) ;
#14365 = CYLINDRICAL_SURFACE ( 'NONE', #4584, 7.500000000000000000 ) ;
#14366 = VERTEX_POINT ( 'NONE', #5116 ) ;
#14367 = VECTOR ( 'NONE', #6422, 1000.000000000000000 ) ;
#14368 = CARTESIAN_POINT ( 'NONE',  ( -71.24615306438114715, 10.00100075456375492, 15.00000000000006928 ) ) ;
#14369 = CARTESIAN_POINT ( 'NONE',  ( -50.24148097183213935, 76.59466308582166505, 15.00000000000009592 ) ) ;
#14370 = VECTOR ( 'NONE', #17271, 1000.000000000000000 ) ;
#14371 = CARTESIAN_POINT ( 'NONE',  ( -86.44887054343442401, 84.22855780814606419, 37.50000000000000000 ) ) ;
#14372 = DIRECTION ( 'NONE',  ( 1.156482317317869999E-16, 0.000000000000000000, 1.000000000000000000 ) ) ;
#14373 = EDGE_LOOP ( 'NONE', ( #1568, #5575, #1270, #16384 ) ) ;
#14374 = LINE ( 'NONE', #8862, #2409 ) ;
#14375 = FACE_OUTER_BOUND ( 'NONE', #9834, .T. ) ;
#14376 = CARTESIAN_POINT ( 'NONE',  ( 5.299999999999998934, 0.000000000000000000, 0.000000000000000000 ) ) ;
#14377 = ORIENTED_EDGE ( 'NONE', *, *, #16934, .F. ) ;
#14378 = VECTOR ( 'NONE', #301, 1000.000000000000000 ) ;
#14379 = CARTESIAN_POINT ( 'NONE',  ( -60.76828531927866095, 74.07097899412299569, 15.00000000000006928 ) ) ;
#14380 = DIRECTION ( 'NONE',  ( 0.000000000000000000, 0.000000000000000000, 1.000000000000000000 ) ) ;
#14381 = VECTOR ( 'NONE', #16040, 1000.000000000000000 ) ;
#14382 = VECTOR ( 'NONE', #16878, 1000.000000000000000 ) ;
#14383 = CARTESIAN_POINT ( 'NONE',  ( -25.66933353722515676, -111.0842361345572158, -5.654315315325675328 ) ) ;
#14384 = ORIENTED_EDGE ( 'NONE', *, *, #9031, .F. ) ;
#14385 = EDGE_CURVE ( 'NONE', #1535, #14470, #9339, .T. ) ;
#14386 = ORIENTED_EDGE ( 'NONE', *, *, #5945, .F. ) ;
#14387 = EDGE_CURVE ( 'NONE', #5064, #2297, #12342, .T. ) ;
#14388 = DIRECTION ( 'NONE',  ( -0.6091372753001471629, -0.7930648017910721936, 0.000000000000000000 ) ) ;
#14389 = VECTOR ( 'NONE', #10576, 1000.000000000000000 ) ;
#14390 = DIRECTION ( 'NONE',  ( 1.000000000000000000, 0.000000000000000000, 0.000000000000000000 ) ) ;
#14391 = CARTESIAN_POINT ( 'NONE',  ( -71.24615306438073503, 129.3815214545637104, 15.00000000000006928 ) ) ;
#14392 = CARTESIAN_POINT ( 'NONE',  ( -71.24615306438106188, 37.38646386522923137, -15.00000000000001421 ) ) ;
#14393 = CARTESIAN_POINT ( 'NONE',  ( -61.89532410461173129, -91.42293623445490880, -41.30285466933271010 ) ) ;
#14394 = ORIENTED_EDGE ( 'NONE', *, *, #6495, .F. ) ;
#14395 = DIRECTION ( 'NONE',  ( -1.000000000000000000, 0.000000000000000000, 0.000000000000000000 ) ) ;
#14396 = AXIS2_PLACEMENT_3D ( 'NONE', #17922, #13824, #13723 ) ;
#14397 = CIRCLE ( 'NONE', #6305, 26.04359719766049608 ) ;
#14398 = DIRECTION ( 'NONE',  ( 0.000000000000000000, 1.000000000000000000, 0.000000000000000000 ) ) ;
#14399 = PRESENTATION_STYLE_ASSIGNMENT (( #1412 ) ) ;
#14400 = CARTESIAN_POINT ( 'NONE',  ( 0.000000000000000000, 0.000000000000000000, 0.000000000000000000 ) ) ;
#14401 = VERTEX_POINT ( 'NONE', #2228 ) ;
#14402 = ADVANCED_FACE ( 'NONE', ( #16529, #14931 ), #18035, .F. ) ;
#14403 = CARTESIAN_POINT ( 'NONE',  ( -42.53669312409158465, -91.08423613455721579, 10.65431531532568599 ) ) ;
#14404 = ADVANCED_FACE ( 'NONE', ( #15223 ), #18137, .T. ) ;
#14405 = CARTESIAN_POINT ( 'NONE',  ( -71.24615306438100504, 50.84170520456370923, -15.00000000000001421 ) ) ;
#14406 = ORIENTED_EDGE ( 'NONE', *, *, #18487, .T. ) ;
#14407 = AXIS2_PLACEMENT_3D ( 'NONE', #12724, #4000, #8402 ) ;
#14408 = DIRECTION ( 'NONE',  ( -0.000000000000000000, -0.000000000000000000, -1.000000000000000000 ) ) ;
#14409 = DIRECTION ( 'NONE',  ( -0.9396926207859084279, 0.3420201433256689905, -4.890320548438449892E-16 ) ) ;
#14410 = ORIENTED_EDGE ( 'NONE', *, *, #9637, .T. ) ;
#14411 = ORIENTED_EDGE ( 'NONE', *, *, #9174, .F. ) ;
#14412 = EDGE_CURVE ( 'NONE', #11452, #6852, #1019, .T. ) ;
#14413 = ADVANCED_FACE ( 'NONE', ( #10734 ), #13732, .T. ) ;
#14414 = CIRCLE ( 'NONE', #1279, 6.500000000000039968 ) ;
#14415 = AXIS2_PLACEMENT_3D ( 'NONE', #7651, #10994, #6687 ) ;
#14416 = EDGE_CURVE ( 'NONE', #1616, #14359, #16624, .T. ) ;
#14417 = VERTEX_POINT ( 'NONE', #10833 ) ;
#14418 = CARTESIAN_POINT ( 'NONE',  ( -71.24615306438103346, 41.41692725456378099, -167.1454815528550739 ) ) ;
#14419 = DIRECTION ( 'NONE',  ( -7.442644330182800165E-16, 1.000000000000000000, 0.000000000000000000 ) ) ;
#14420 = DIRECTION ( 'NONE',  ( -0.000000000000000000, -0.000000000000000000, 1.000000000000000000 ) ) ;
#14421 = VECTOR ( 'NONE', #2361, 1000.000000000000000 ) ;
#14422 = CYLINDRICAL_SURFACE ( 'NONE', #3010, 20.99999999999999645 ) ;
#14423 = EDGE_CURVE ( 'NONE', #857, #15190, #8681, .T. ) ;
#14424 = DIRECTION ( 'NONE',  ( 0.3420201433256481738, 0.9396926207859158664, -0.000000000000000000 ) ) ;
#14425 = ORIENTED_EDGE ( 'NONE', *, *, #18069, .T. ) ;
#14426 = ADVANCED_FACE ( 'NONE', ( #16711 ), #6434, .T. ) ;
#14427 = ADVANCED_FACE ( 'NONE', ( #14848 ), #7740, .F. ) ;
#14428 = CARTESIAN_POINT ( 'NONE',  ( -67.88623620617454435, 84.15481808402788033, 15.00000000000006928 ) ) ;
#14429 = ORIENTED_EDGE ( 'NONE', *, *, #16581, .F. ) ;
#14430 = CARTESIAN_POINT ( 'NONE',  ( 5.233202738124664855, -111.0842361345572158, 57.00000000000000000 ) ) ;
#14431 = CONICAL_SURFACE ( 'NONE', #15620, 4.025000000000000355, 0.7853981633974482790 ) ;
#14432 = VECTOR ( 'NONE', #18084, 1000.000000000000000 ) ;
#14433 = EDGE_CURVE ( 'NONE', #16418, #2884, #6329, .T. ) ;
#14434 = DIRECTION ( 'NONE',  ( 0.000000000000000000, 1.000000000000000000, 0.000000000000000000 ) ) ;
#14435 = VERTEX_POINT ( 'NONE', #4943 ) ;
#14436 = DIRECTION ( 'NONE',  ( -5.204170427930409450E-16, 0.000000000000000000, 1.000000000000000000 ) ) ;
#14437 = ORIENTED_EDGE ( 'NONE', *, *, #9629, .F. ) ;
#14438 = EDGE_CURVE ( 'NONE', #13404, #3088, #16340, .T. ) ;
#14439 = VECTOR ( 'NONE', #12472, 1000.000000000000000 ) ;
#14440 = EDGE_CURVE ( 'NONE', #18243, #13143, #4191, .T. ) ;
#14441 = ORIENTED_EDGE ( 'NONE', *, *, #2414, .F. ) ;
#14442 = CIRCLE ( 'NONE', #3362, 12.50000000000000355 ) ;
#14443 = CIRCLE ( 'NONE', #2806, 22.04359719766050318 ) ;
#14444 = CIRCLE ( 'NONE', #3682, 2.168074330098676672 ) ;
#14445 = CARTESIAN_POINT ( 'NONE',  ( 5.233202738124664855, -46.83756720124470263, -115.7605492041889619 ) ) ;
#14446 = DIRECTION ( 'NONE',  ( -1.000000000000000000, 0.000000000000000000, 0.000000000000000000 ) ) ;
#14447 = DIRECTION ( 'NONE',  ( 0.000000000000000000, 1.000000000000000000, 0.000000000000000000 ) ) ;
#14448 = VERTEX_POINT ( 'NONE', #8409 ) ;
#14449 = ORIENTED_EDGE ( 'NONE', *, *, #9799, .F. ) ;
#14450 = CARTESIAN_POINT ( 'NONE',  ( -68.99615306438089135, 86.21815738166266385, -167.1454815528550739 ) ) ;
#14451 = LINE ( 'NONE', #4257, #9591 ) ;
#14452 = DIRECTION ( 'NONE',  ( -1.000000000000000000, -3.016910393003147592E-15, 0.000000000000000000 ) ) ;
#14453 = ORIENTED_EDGE ( 'NONE', *, *, #1506, .F. ) ;
#14454 = EDGE_CURVE ( 'NONE', #12621, #3501, #12635, .T. ) ;
#14455 = DIRECTION ( 'NONE',  ( 0.000000000000000000, 0.000000000000000000, 1.000000000000000000 ) ) ;
#14456 = ORIENTED_EDGE ( 'NONE', *, *, #7501, .T. ) ;
#14457 = VECTOR ( 'NONE', #10423, 1000.000000000000000 ) ;
#14458 = ORIENTED_EDGE ( 'NONE', *, *, #16595, .F. ) ;
#14459 = EDGE_LOOP ( 'NONE', ( #7080, #153, #8621, #4941 ) ) ;
#14460 = CYLINDRICAL_SURFACE ( 'NONE', #10273, 81.86696747278379860 ) ;
#14461 = DIRECTION ( 'NONE',  ( 1.000000000000000000, 0.000000000000000000, -0.000000000000000000 ) ) ;
#14462 = CARTESIAN_POINT ( 'NONE',  ( -57.08002265617300708, 84.22855780814606419, -167.1454815528550739 ) ) ;
#14463 = EDGE_LOOP ( 'NONE', ( #17636, #391, #10189, #8632, #14453, #4416 ) ) ;
#14464 = AXIS2_PLACEMENT_3D ( 'NONE', #14744, #15879, #11675 ) ;
#14465 = CARTESIAN_POINT ( 'NONE',  ( -68.99615306438106188, 29.66948968166269296, 15.00000000000006928 ) ) ;
#14467 = AXIS2_PLACEMENT_3D ( 'NONE', #10487, #4767, #6262 ) ;
#14466 = CYLINDRICAL_SURFACE ( 'NONE', #17296, 11.04359719766049430 ) ;
#14468 = CARTESIAN_POINT ( 'NONE',  ( -54.95363092160842911, 73.63336328296981037, -167.1454815528550739 ) ) ;
#14469 = DIRECTION ( 'NONE',  ( 0.000000000000000000, 0.000000000000000000, 1.000000000000000000 ) ) ;
#14470 = VERTEX_POINT ( 'NONE', #6907 ) ;
#14471 = CYLINDRICAL_SURFACE ( 'NONE', #6920, 4.599999999999992539 ) ;
#14472 = CARTESIAN_POINT ( 'NONE',  ( -71.24615306438094819, 65.66079771522920794, -167.1454815528550739 ) ) ;
#14473 = FACE_OUTER_BOUND ( 'NONE', #6968, .T. ) ;
#14474 = ORIENTED_EDGE ( 'NONE', *, *, #7769, .F. ) ;
#14475 = VECTOR ( 'NONE', #6190, 1000.000000000000000 ) ;
#14476 = DIRECTION ( 'NONE',  ( 1.000000000000000000, 0.000000000000000000, 0.000000000000000000 ) ) ;
#14477 = AXIS2_PLACEMENT_3D ( 'NONE', #1457, #7160, #5113 ) ;
#14478 = DIRECTION ( 'NONE',  ( -0.000000000000000000, -1.000000000000000000, 0.000000000000000000 ) ) ;
#14479 = CIRCLE ( 'NONE', #3400, 4.025000000000000355 ) ;
#14480 = ORIENTED_EDGE ( 'NONE', *, *, #9063, .F. ) ;
#14481 = CIRCLE ( 'NONE', #15967, 4.025000000000000355 ) ;
#14482 = VERTEX_POINT ( 'NONE', #18507 ) ;
#14484 = EDGE_CURVE ( 'NONE', #11504, #1708, #8977, .T. ) ;
#14483 = CYLINDRICAL_SURFACE ( 'NONE', #3364, 4.599999999999992539 ) ;
#14485 = CIRCLE ( 'NONE', #7910, 10.24900000000000766 ) ;
#14486 = DIRECTION ( 'NONE',  ( 0.000000000000000000, 0.000000000000000000, 1.000000000000000000 ) ) ;
#14487 = CARTESIAN_POINT ( 'NONE',  ( -71.24615306438103346, 40.52805651522925245, -167.1454815528550739 ) ) ;
#14488 = DIRECTION ( 'NONE',  ( 1.000000000000000000, 2.062304371594500494E-16, 0.000000000000000000 ) ) ;
#14489 = ORIENTED_EDGE ( 'NONE', *, *, #1307, .T. ) ;
#14490 = AXIS2_PLACEMENT_3D ( 'NONE', #12231, #16525, #13931 ) ;
#14491 = CARTESIAN_POINT ( 'NONE',  ( 124.5381772159375942, -111.0842361345572158, -6.999999999999985789 ) ) ;
#14492 = CIRCLE ( 'NONE', #6729, 26.04359719766049608 ) ;
#14493 = DIRECTION ( 'NONE',  ( 0.9396926207859065405, 0.3420201433256737089, 0.000000000000000000 ) ) ;
#14494 = CARTESIAN_POINT ( 'NONE',  ( 0.000000000000000000, 0.000000000000000000, 0.000000000000000000 ) ) ;
#14495 = CIRCLE ( 'NONE', #14215, 12.50000000000000355 ) ;
#14496 = DIRECTION ( 'NONE',  ( 1.000000000000000000, 0.000000000000000000, 0.000000000000000000 ) ) ;
#14497 = VERTEX_POINT ( 'NONE', #8595 ) ;
#14498 = DIRECTION ( 'NONE',  ( -5.204170427930409450E-16, 0.000000000000000000, 1.000000000000000000 ) ) ;
#14499 = LINE ( 'NONE', #3444, #3292 ) ;
#14500 = ORIENTED_EDGE ( 'NONE', *, *, #15718, .F. ) ;
#14501 = FACE_OUTER_BOUND ( 'NONE', #7625, .T. ) ;
#14502 = DIRECTION ( 'NONE',  ( 1.000000000000000000, -0.000000000000000000, -0.000000000000000000 ) ) ;
#14503 = ORIENTED_EDGE ( 'NONE', *, *, #17842, .F. ) ;
#14504 = ORIENTED_EDGE ( 'NONE', *, *, #12631, .F. ) ;
#14505 =( GEOMETRIC_REPRESENTATION_CONTEXT ( 3 ) GLOBAL_UNCERTAINTY_ASSIGNED_CONTEXT ( ( #14876 ) ) GLOBAL_UNIT_ASSIGNED_CONTEXT ( ( #3998, #5393, #7933 ) ) REPRESENTATION_CONTEXT ( 'NONE', 'WORKASPACE' ) );
#14506 = CIRCLE ( 'NONE', #5243, 4.600000000000006750 ) ;
#14508 = EDGE_CURVE ( 'NONE', #1462, #2272, #11227, .T. ) ;
#14507 = ORIENTED_EDGE ( 'NONE', *, *, #13149, .F. ) ;
#14509 = CARTESIAN_POINT ( 'NONE',  ( -71.24615306438076345, 131.6342433652292243, -15.00000000000001421 ) ) ;
#14510 = DIRECTION ( 'NONE',  ( 0.000000000000000000, 1.000000000000000000, 0.000000000000000000 ) ) ;
#14511 = LINE ( 'NONE', #10203, #558 ) ;
#14512 = DIRECTION ( 'NONE',  ( 0.000000000000000000, 5.551115123125748189E-17, 1.000000000000000000 ) ) ;
#14513 = LINE ( 'NONE', #11440, #4812 ) ;
#14514 = EDGE_LOOP ( 'NONE', ( #11844, #17490, #5244, #9111, #14294, #9458, #9976 ) ) ;
#14515 = PLANE ( 'NONE',  #4231 ) ;
#14516 = EDGE_CURVE ( 'NONE', #14266, #16358, #1397, .T. ) ;
#14517 = CARTESIAN_POINT ( 'NONE',  ( -66.40868851600848188, 112.0764521540501875, 25.00000000000000355 ) ) ;
#14518 = CIRCLE ( 'NONE', #1034, 11.04359719766049430 ) ;
#14519 = FACE_OUTER_BOUND ( 'NONE', #13004, .T. ) ;
#14520 = ORIENTED_EDGE ( 'NONE', *, *, #828, .F. ) ;
#14521 = DIRECTION ( 'NONE',  ( 0.9396926207859084279, 0.3420201433256686574, 0.000000000000000000 ) ) ;
#14522 = DIRECTION ( 'NONE',  ( -0.000000000000000000, -0.000000000000000000, -1.000000000000000000 ) ) ;
#14523 = ADVANCED_FACE ( 'NONE', ( #1117 ), #4007, .T. ) ;
#14524 = ADVANCED_FACE ( 'NONE', ( #2510 ), #12532, .T. ) ;
#14525 = EDGE_LOOP ( 'NONE', ( #93, #10676, #6187, #11932 ) ) ;
#14526 = EDGE_CURVE ( 'NONE', #17119, #7091, #9809, .T. ) ;
#14527 = DIRECTION ( 'NONE',  ( 0.000000000000000000, 1.000000000000000000, 0.000000000000000000 ) ) ;
#14528 = DIRECTION ( 'NONE',  ( 1.156482317317869999E-16, 0.000000000000000000, 1.000000000000000000 ) ) ;
#14529 = CARTESIAN_POINT ( 'NONE',  ( -107.5676225674731938, 110.5691553257988460, 26.35917033480641436 ) ) ;
#14530 = ORIENTED_EDGE ( 'NONE', *, *, #2053, .T. ) ;
#14531 = ORIENTED_EDGE ( 'NONE', *, *, #14387, .T. ) ;
#14532 = ADVANCED_FACE ( 'NONE', ( #18332 ), #4292, .F. ) ;
#14533 = DIRECTION ( 'NONE',  ( -0.000000000000000000, -0.000000000000000000, -1.000000000000000000 ) ) ;
#14534 = DIRECTION ( 'NONE',  ( 0.000000000000000000, 0.000000000000000000, 1.000000000000000000 ) ) ;
#14535 = DIRECTION ( 'NONE',  ( 0.3420201433256687684, 0.9396926207859084279, -0.000000000000000000 ) ) ;
#14536 = ADVANCED_FACE ( 'NONE', ( #15714 ), #11128, .T. ) ;
#14537 = CARTESIAN_POINT ( 'NONE',  ( -66.02736529514692165, 75.49957964911740760, 15.00000000000006928 ) ) ;
#14538 = EDGE_CURVE ( 'NONE', #616, #18359, #9583, .T. ) ;
#14539 = EDGE_LOOP ( 'NONE', ( #16895, #10662, #7162, #926 ) ) ;
#14540 = DIRECTION ( 'NONE',  ( 0.000000000000000000, 0.000000000000000000, -1.000000000000000000 ) ) ;
#14541 = ORIENTED_EDGE ( 'NONE', *, *, #16691, .T. ) ;
#14542 = EDGE_CURVE ( 'NONE', #11331, #2191, #7099, .T. ) ;
#14543 = ORIENTED_EDGE ( 'NONE', *, *, #16329, .T. ) ;
#14544 = ADVANCED_FACE ( 'NONE', ( #5403 ), #11500, .F. ) ;
#14545 = ORIENTED_EDGE ( 'NONE', *, *, #14303, .T. ) ;
#14546 = EDGE_CURVE ( 'NONE', #7091, #15955, #3909, .T. ) ;
#14547 = LINE ( 'NONE', #4793, #9090 ) ;
#14548 = EDGE_CURVE ( 'NONE', #6499, #15744, #3861, .T. ) ;
#14549 = CARTESIAN_POINT ( 'NONE',  ( -68.99615306438106188, 27.14275288813031040, -15.00000000000001421 ) ) ;
#14550 = ORIENTED_EDGE ( 'NONE', *, *, #14863, .F. ) ;
#14551 = LINE ( 'NONE', #14202, #13738 ) ;
#14552 = CARTESIAN_POINT ( 'NONE',  ( -57.08002265617300708, 84.22855780814606419, -62.50000000000000000 ) ) ;
#14553 = DIRECTION ( 'NONE',  ( 1.000000000000000000, 0.000000000000000000, 0.000000000000000000 ) ) ;
#14554 = CARTESIAN_POINT ( 'NONE',  ( -68.99615306438067819, 142.7668250816626596, -15.00000000000001421 ) ) ;
#14555 = EDGE_LOOP ( 'NONE', ( #15918, #2506, #9139, #486, #9209, #11007, #13988, #13266, #2267, #11334 ) ) ;
#14556 = CARTESIAN_POINT ( 'NONE',  ( -68.99615306438089135, 80.54982793813027797, 15.00000000000006928 ) ) ;
#14557 = LINE ( 'NONE', #12992, #10815 ) ;
#14558 = DIRECTION ( 'NONE',  ( 1.156482317317869999E-16, 0.000000000000000000, 1.000000000000000000 ) ) ;
#14559 = ORIENTED_EDGE ( 'NONE', *, *, #18438, .F. ) ;
#14560 = DIRECTION ( 'NONE',  ( 0.000000000000000000, 0.000000000000000000, 1.000000000000000000 ) ) ;
#14561 = DIRECTION ( 'NONE',  ( -0.9396926207859084279, 0.3420201433256689905, 1.086737899652989769E-16 ) ) ;
#14562 = ORIENTED_EDGE ( 'NONE', *, *, #14075, .T. ) ;
#14563 = ORIENTED_EDGE ( 'NONE', *, *, #871, .F. ) ;
#14564 = ORIENTED_EDGE ( 'NONE', *, *, #14964, .F. ) ;
#14565 = DIRECTION ( 'NONE',  ( 1.000000000000000000, 0.000000000000000000, 0.000000000000000000 ) ) ;
#14566 = CARTESIAN_POINT ( 'NONE',  ( 0.000000000000000000, 0.000000000000000000, 0.000000000000000000 ) ) ;
#14567 = DIRECTION ( 'NONE',  ( 0.000000000000000000, 0.000000000000000000, 1.000000000000000000 ) ) ;
#14568 =( NAMED_UNIT ( * ) PLANE_ANGLE_UNIT ( ) SI_UNIT ( $, .RADIAN. ) );
#14569 = CARTESIAN_POINT ( 'NONE',  ( -49.93060289285580922, 91.57211267264388255, 15.00000000000006928 ) ) ;
#14570 = CARTESIAN_POINT ( 'NONE',  ( -65.41598826576338865, 91.10542963993673027, 15.00000000000006928 ) ) ;
#14571 = ORIENTED_EDGE ( 'NONE', *, *, #11797, .F. ) ;
#14572 = FACE_OUTER_BOUND ( 'NONE', #16266, .T. ) ;
#14573 = CARTESIAN_POINT ( 'NONE',  ( 5.299999999999996270, -2.442490654175344586E-16, -4.400000000000027889 ) ) ;
#14574 = CARTESIAN_POINT ( 'NONE',  ( -68.99615306438100504, 45.99230878813026635, 15.00000000000006928 ) ) ;
#14575 = DIRECTION ( 'NONE',  ( 1.000000000000000000, 0.000000000000000000, 0.000000000000000000 ) ) ;
#14576 = CARTESIAN_POINT ( 'NONE',  ( -36.89464699146818560, 90.18382313193718858, 57.91473613501618445 ) ) ;
#14577 = DIRECTION ( 'NONE',  ( 0.000000000000000000, 0.000000000000000000, 1.000000000000000000 ) ) ;
#14578 = VERTEX_POINT ( 'NONE', #15318 ) ;
#14579 = EDGE_CURVE ( 'NONE', #13177, #8500, #11312, .T. ) ;
#14580 = FACE_OUTER_BOUND ( 'NONE', #10107, .T. ) ;
#14581 = DIRECTION ( 'NONE',  ( 0.9396926207859078728, 0.3420201433256701007, 4.890320548438446933E-16 ) ) ;
#14582 = VERTEX_POINT ( 'NONE', #4453 ) ;
#14583 = ORIENTED_EDGE ( 'NONE', *, *, #14030, .T. ) ;
#14584 = EDGE_CURVE ( 'NONE', #11293, #4896, #3320, .T. ) ;
#14585 = TOROIDAL_SURFACE ( 'NONE', #10698, 2.168074330099288183, 5.000000000000000000 ) ;
#14586 = EDGE_LOOP ( 'NONE', ( #16468, #12535, #5312 ) ) ;
#14587 = CARTESIAN_POINT ( 'NONE',  ( 0.000000000000000000, 5.629165124598801917, 3.250000000000037748 ) ) ;
#14588 = CARTESIAN_POINT ( 'NONE',  ( -71.24615306438093398, 69.69126110456375045, -15.00000000000001421 ) ) ;
#14589 = CARTESIAN_POINT ( 'NONE',  ( -47.88529808651028929, 78.55081803573747834, -167.1454815528550739 ) ) ;
#14590 = CARTESIAN_POINT ( 'NONE',  ( 98.04320049944426785, 84.22855780814606419, 52.11995643276230794 ) ) ;
#14591 = CARTESIAN_POINT ( 'NONE',  ( 276.3098885457529832, -32.62665103886256190, 7.000000000000010658 ) ) ;
#14592 = CARTESIAN_POINT ( 'NONE',  ( -198.5768363665157494, 84.22855780814606419, 62.50000000000001421 ) ) ;
#14593 = LINE ( 'NONE', #8547, #9920 ) ;
#14594 = ORIENTED_EDGE ( 'NONE', *, *, #16707, .T. ) ;
#14595 = PLANE ( 'NONE',  #11115 ) ;
#14596 = CARTESIAN_POINT ( 'NONE',  ( -67.59262256747315689, 129.5689604715732912, 15.00000000000005862 ) ) ;
#14597 = CARTESIAN_POINT ( 'NONE',  ( -68.99615306438097662, 58.55867938813025830, -167.1454815528550739 ) ) ;
#14598 = VECTOR ( 'NONE', #5142, 1000.000000000000000 ) ;
#14599 = ORIENTED_EDGE ( 'NONE', *, *, #15781, .T. ) ;
#14600 = DIRECTION ( 'NONE',  ( -0.9396926207859171987, 0.3420201433256444545, 0.000000000000000000 ) ) ;
#14601 = CARTESIAN_POINT ( 'NONE',  ( -47.03642545851250389, 84.22855780814606419, -62.50000000000000000 ) ) ;
#14602 = ORIENTED_EDGE ( 'NONE', *, *, #1705, .T. ) ;
#14603 = VERTEX_POINT ( 'NONE', #14731 ) ;
#14604 = EDGE_CURVE ( 'NONE', #17887, #11425, #12273, .T. ) ;
#14605 = CARTESIAN_POINT ( 'NONE',  ( -68.99615306438109030, 17.10311908166270456, 15.00000000000006928 ) ) ;
#14606 = VECTOR ( 'NONE', #17301, 1000.000000000000000 ) ;
#14607 = CARTESIAN_POINT ( 'NONE',  ( -107.5676225674731654, 57.88796029049330372, -22.35917033480641791 ) ) ;
#14608 = CARTESIAN_POINT ( 'NONE',  ( 45.30000000000000426, 0.000000000000000000, 0.000000000000000000 ) ) ;
#14609 = ORIENTED_EDGE ( 'NONE', *, *, #18201, .T. ) ;
#14610 = ORIENTED_EDGE ( 'NONE', *, *, #4337, .T. ) ;
#14611 = CARTESIAN_POINT ( 'NONE',  ( -71.24615306438111872, 18.53690796522925055, 15.00000000000006928 ) ) ;
#14612 = DIRECTION ( 'NONE',  ( 0.000000000000000000, -1.000000000000000000, 0.000000000000000000 ) ) ;
#14613 = DIRECTION ( 'NONE',  ( 0.000000000000000000, 1.000000000000000000, -0.000000000000000000 ) ) ;
#14614 = DIRECTION ( 'NONE',  ( 0.000000000000000000, 0.000000000000000000, 1.000000000000000000 ) ) ;
#14615 = ORIENTED_EDGE ( 'NONE', *, *, #12121, .F. ) ;
#14616 = ADVANCED_FACE ( 'NONE', ( #7446 ), #4717, .T. ) ;
#14617 = CARTESIAN_POINT ( 'NONE',  ( -66.39376235201207521, 88.50596986196454452, -15.00000000000001243 ) ) ;
#14618 = ORIENTED_EDGE ( 'NONE', *, *, #14538, .T. ) ;
#14619 = CARTESIAN_POINT ( 'NONE',  ( 95.45835937779683888, -32.62665103886256190, 7.000000000000010658 ) ) ;
#14620 = ORIENTED_EDGE ( 'NONE', *, *, #12825, .T. ) ;
#14621 = VECTOR ( 'NONE', #3036, 1000.000000000000000 ) ;
#14622 = TOROIDAL_SURFACE ( 'NONE', #3564, 2.168074330098679336, 5.000000000000000000 ) ;
#14623 = ORIENTED_EDGE ( 'NONE', *, *, #12257, .T. ) ;
#14624 = ADVANCED_FACE ( 'NONE', ( #13253, #17194 ), #9044, .F. ) ;
#14625 = EDGE_CURVE ( 'NONE', #5721, #6138, #11584, .T. ) ;
#14626 = SURFACE_STYLE_FILL_AREA ( #5849 ) ;
#14627 = CYLINDRICAL_SURFACE ( 'NONE', #7866, 4.600000000000006750 ) ;
#14628 = EDGE_LOOP ( 'NONE', ( #16965, #3202, #8081, #12655 ) ) ;
#14629 = CARTESIAN_POINT ( 'NONE',  ( -46.03642545851250389, 84.22855780814606419, -35.00000000000000000 ) ) ;
#14630 = DIRECTION ( 'NONE',  ( -0.000000000000000000, -0.000000000000000000, -1.000000000000000000 ) ) ;
#14631 = AXIS2_PLACEMENT_3D ( 'NONE', #2567, #13780, #6765 ) ;
#14632 = FACE_OUTER_BOUND ( 'NONE', #4345, .T. ) ;
#14633 = ORIENTED_EDGE ( 'NONE', *, *, #478, .T. ) ;
#14634 = EDGE_CURVE ( 'NONE', #17089, #11153, #18222, .T. ) ;
#14635 = DIRECTION ( 'NONE',  ( 1.000000000000000000, 0.000000000000000000, 3.771137991253928573E-16 ) ) ;
#14636 = AXIS2_PLACEMENT_3D ( 'NONE', #380, #11798, #17486 ) ;
#14637 = VECTOR ( 'NONE', #2611, 1000.000000000000114 ) ;
#14638 = EDGE_CURVE ( 'NONE', #11938, #12123, #10437, .T. ) ;
#14639 = DIRECTION ( 'NONE',  ( -0.000000000000000000, -0.000000000000000000, -1.000000000000000000 ) ) ;
#14640 = DIRECTION ( 'NONE',  ( -1.000000000000000000, 3.016910393003142859E-15, 0.000000000000000000 ) ) ;
#14641 = ORIENTED_EDGE ( 'NONE', *, *, #6143, .T. ) ;
#14642 = EDGE_CURVE ( 'NONE', #14698, #16861, #4379, .T. ) ;
#14643 = DIRECTION ( 'NONE',  ( 0.000000000000000000, 0.000000000000000000, 1.000000000000000000 ) ) ;
#14644 = EDGE_CURVE ( 'NONE', #13790, #16158, #11847, .T. ) ;
#14645 = CIRCLE ( 'NONE', #11079, 29.36884788726140627 ) ;
#14646 = DIRECTION ( 'NONE',  ( 0.000000000000000000, 0.000000000000000000, -1.000000000000000000 ) ) ;
#14647 = EDGE_LOOP ( 'NONE', ( #3257, #973, #11928, #11626 ) ) ;
#14648 = CIRCLE ( 'NONE', #8678, 9.197489084949710403 ) ;
#14649 = VERTEX_POINT ( 'NONE', #16128 ) ;
#14650 = ADVANCED_FACE ( 'NONE', ( #7638 ), #13162, .F. ) ;
#14651 = AXIS2_PLACEMENT_3D ( 'NONE', #186, #4390, #10098 ) ;
#14652 = CONICAL_SURFACE ( 'NONE', #8040, 7.500000000000007105, 0.1302312384721128480 ) ;
#14653 = VERTEX_POINT ( 'NONE', #8950 ) ;
#14654 = DIRECTION ( 'NONE',  ( 1.000000000000000000, 0.000000000000000000, 0.000000000000000000 ) ) ;
#14655 = LINE ( 'NONE', #1844, #18086 ) ;
#14656 = CARTESIAN_POINT ( 'NONE',  ( -68.99615306438072082, 133.9569029881302811, 15.00000000000006928 ) ) ;
#14657 = CARTESIAN_POINT ( 'NONE',  ( -71.24615306438070661, 187.7866419848965052, 15.00000000000006928 ) ) ;
#14658 = LINE ( 'NONE', #3166, #2830 ) ;
#14659 = ORIENTED_EDGE ( 'NONE', *, *, #7916, .T. ) ;
#14660 = DIRECTION ( 'NONE',  ( -1.000000000000000000, 0.000000000000000000, 0.000000000000000000 ) ) ;
#14661 = CARTESIAN_POINT ( 'NONE',  ( -65.06546592763146464, -96.08423613455721579, 45.05044770573184110 ) ) ;
#14662 = LINE ( 'NONE', #17549, #13512 ) ;
#14663 = CARTESIAN_POINT ( 'NONE',  ( -36.12242140784905331, 86.19059744224306030, 69.75578550468861749 ) ) ;
#14664 = AXIS2_PLACEMENT_3D ( 'NONE', #10907, #15185, #3785 ) ;
#14665 = AXIS2_PLACEMENT_3D ( 'NONE', #791, #12200, #17892 ) ;
#14666 = DIRECTION ( 'NONE',  ( -0.000000000000000000, -1.000000000000000000, -0.000000000000000000 ) ) ;
#14667 = ORIENTED_EDGE ( 'NONE', *, *, #10651, .T. ) ;
#14668 = CARTESIAN_POINT ( 'NONE',  ( -66.32174931794583017, 59.21973273998174392, 25.00000000000000711 ) ) ;
#14669 = CARTESIAN_POINT ( 'NONE',  ( -36.10496011515223103, 82.51445519007735641, 55.19436440210437667 ) ) ;
#14670 = ORIENTED_EDGE ( 'NONE', *, *, #4239, .T. ) ;
#14671 = ORIENTED_EDGE ( 'NONE', *, *, #6117, .T. ) ;
#14672 = ORIENTED_EDGE ( 'NONE', *, *, #10980, .T. ) ;
#14673 = CIRCLE ( 'NONE', #1548, 4.599999999999999645 ) ;
#14674 = AXIS2_PLACEMENT_3D ( 'NONE', #112, #14424, #7314 ) ;
#14675 = LINE ( 'NONE', #11607, #13290 ) ;
#14676 = CARTESIAN_POINT ( 'NONE',  ( -71.24615306438109030, 28.85055665456373575, -167.1454815528550739 ) ) ;
#14677 = CARTESIAN_POINT ( 'NONE',  ( -77.53465414598844063, 79.27196096192940900, 56.85026520973028141 ) ) ;
#14678 = FACE_OUTER_BOUND ( 'NONE', #2941, .T. ) ;
#14679 = CARTESIAN_POINT ( 'NONE',  ( -64.18632899337946185, 107.0896764944433954, 92.50000000000000000 ) ) ;
#14680 = LINE ( 'NONE', #13297, #12729 ) ;
#14681 = CARTESIAN_POINT ( 'NONE',  ( -57.08002265617300708, 84.22855780814606419, 37.50000000000000000 ) ) ;
#14682 = ORIENTED_EDGE ( 'NONE', *, *, #10891, .T. ) ;
#14683 = CARTESIAN_POINT ( 'NONE',  ( -207.6107609645051753, 84.22855780814606419, 74.79357405616491405 ) ) ;
#14684 = LINE ( 'NONE', #14596, #10252 ) ;
#14685 = CARTESIAN_POINT ( 'NONE',  ( -47.59681378869034774, 80.34130291867735707, -15.00000000000001421 ) ) ;
#14686 = ORIENTED_EDGE ( 'NONE', *, *, #16444, .T. ) ;
#14687 = AXIS2_PLACEMENT_3D ( 'NONE', #16334, #14925, #10826 ) ;
#14688 = CARTESIAN_POINT ( 'NONE',  ( -70.71978124295708312, -111.0842361345572158, 28.18308811886538479 ) ) ;
#14689 = VECTOR ( 'NONE', #11327, 1000.000000000000000 ) ;
#14690 = CARTESIAN_POINT ( 'NONE',  ( -49.65031598894605480, 92.07579602767992810, -15.00000000000001421 ) ) ;
#14691 = EDGE_LOOP ( 'NONE', ( #46, #18471, #13690, #15848, #11900 ) ) ;
#14692 = ORIENTED_EDGE ( 'NONE', *, *, #349, .F. ) ;
#14693 = VECTOR ( 'NONE', #4339, 1000.000000000000000 ) ;
#14694 = DIRECTION ( 'NONE',  ( 1.000000000000000000, 0.000000000000000000, 5.077734830647299712E-16 ) ) ;
#14695 = CARTESIAN_POINT ( 'NONE',  ( -36.44155368744860368, 56.74635804676025685, -22.50216374311546019 ) ) ;
#14696 = EDGE_CURVE ( 'NONE', #9888, #3197, #13343, .T. ) ;
#14697 = PLANE ( 'NONE',  #8136 ) ;
#14698 = VERTEX_POINT ( 'NONE', #8867 ) ;
#14699 = AXIS2_PLACEMENT_3D ( 'NONE', #5469, #15398, #5366 ) ;
#14700 = AXIS2_PLACEMENT_3D ( 'NONE', #15579, #12594, #11286 ) ;
#14701 = ORIENTED_EDGE ( 'NONE', *, *, #13648, .T. ) ;
#14702 = CARTESIAN_POINT ( 'NONE',  ( -75.23640716657477867, 71.26406042838995347, 97.49999999999998579 ) ) ;
#14703 = CARTESIAN_POINT ( 'NONE',  ( -67.00421887699711476, 86.78830982163884755, 15.00000000000006928 ) ) ;
#14704 = DIRECTION ( 'NONE',  ( 0.000000000000000000, 1.000000000000000000, 0.000000000000000000 ) ) ;
#14705 = DIRECTION ( 'NONE',  ( -0.000000000000000000, 1.000000000000000000, -0.000000000000000000 ) ) ;
#14706 = VERTEX_POINT ( 'NONE', #12998 ) ;
#14707 = CARTESIAN_POINT ( 'NONE',  ( -36.44155368744860368, 56.74635804676025685, -22.50216374311546019 ) ) ;
#14708 = EDGE_LOOP ( 'NONE', ( #17997, #3324, #13396, #15830 ) ) ;
#14709 = DIRECTION ( 'NONE',  ( 0.000000000000000000, 0.000000000000000000, -1.000000000000000000 ) ) ;
#14710 = VERTEX_POINT ( 'NONE', #15869 ) ;
#14711 = AXIS2_PLACEMENT_3D ( 'NONE', #7129, #16850, #9757 ) ;
#14712 = VERTEX_POINT ( 'NONE', #3059 ) ;
#14713 = VECTOR ( 'NONE', #17398, 1000.000000000000000 ) ;
#14714 = EDGE_LOOP ( 'NONE', ( #817, #1136, #9475, #14822 ) ) ;
#14715 = DIRECTION ( 'NONE',  ( 0.9396926207859157554, 0.3420201433256481738, 4.890320548438487362E-16 ) ) ;
#14716 = VECTOR ( 'NONE', #15204, 1000.000000000000000 ) ;
#14717 = ORIENTED_EDGE ( 'NONE', *, *, #7000, .T. ) ;
#14718 = ADVANCED_FACE ( 'NONE', ( #1660 ), #14652, .T. ) ;
#14719 = FACE_OUTER_BOUND ( 'NONE', #16602, .T. ) ;
#14720 = DIRECTION ( 'NONE',  ( -0.9396926207859171987, 0.3420201433256445100, -4.890320548438495251E-16 ) ) ;
#14721 = CARTESIAN_POINT ( 'NONE',  ( -107.5926225674731853, 110.5691553257988460, 30.38417033480641294 ) ) ;
#14722 = ORIENTED_EDGE ( 'NONE', *, *, #17152, .T. ) ;
#14723 = DIRECTION ( 'NONE',  ( 1.000000000000000000, 0.000000000000000000, 5.077734830647306615E-16 ) ) ;
#14724 = AXIS2_PLACEMENT_3D ( 'NONE', #6702, #4274, #11389 ) ;
#14725 = VECTOR ( 'NONE', #16348, 1000.000000000000114 ) ;
#14726 = DIRECTION ( 'NONE',  ( 0.3420201433256854218, 0.9396926207859023217, -0.000000000000000000 ) ) ;
#14727 = LINE ( 'NONE', #4633, #3334 ) ;
#14728 = EDGE_LOOP ( 'NONE', ( #9793, #2931, #9926, #15938 ) ) ;
#14729 = EDGE_CURVE ( 'NONE', #15101, #8820, #8777, .T. ) ;
#14730 = FACE_OUTER_BOUND ( 'NONE', #15547, .T. ) ;
#14731 = CARTESIAN_POINT ( 'NONE',  ( -107.5926225674731853, 50.58224449241411236, -25.00000000000000000 ) ) ;
#14732 = ORIENTED_EDGE ( 'NONE', *, *, #14755, .F. ) ;
#14733 = ORIENTED_EDGE ( 'NONE', *, *, #6772, .T. ) ;
#14734 = EDGE_CURVE ( 'NONE', #3722, #13457, #17450, .T. ) ;
#14735 = VECTOR ( 'NONE', #5479, 1000.000000000000000 ) ;
#14736 = ORIENTED_EDGE ( 'NONE', *, *, #17597, .F. ) ;
#14737 = ADVANCED_FACE ( 'NONE', ( #3159 ), #1740, .F. ) ;
#14738 = DIRECTION ( 'NONE',  ( 0.000000000000000000, 0.000000000000000000, 1.000000000000000000 ) ) ;
#14739 = EDGE_CURVE ( 'NONE', #3439, #7034, #4640, .T. ) ;
#14740 = ORIENTED_EDGE ( 'NONE', *, *, #7904, .T. ) ;
#14741 = DIRECTION ( 'NONE',  ( 0.000000000000000000, 0.000000000000000000, 1.000000000000000000 ) ) ;
#14742 = FACE_OUTER_BOUND ( 'NONE', #1417, .T. ) ;
#14743 = LINE ( 'NONE', #7375, #16506 ) ;
#14744 = CARTESIAN_POINT ( 'NONE',  ( -71.24615306438089135, 85.39922435456371375, -167.1454815528550739 ) ) ;
#14745 = ORIENTED_EDGE ( 'NONE', *, *, #727, .T. ) ;
#14746 = AXIS2_PLACEMENT_3D ( 'NONE', #15768, #17176, #5755 ) ;
#14747 = CARTESIAN_POINT ( 'NONE',  ( 4.699999999999995737, 3.752776749732559924, -6.500000000000061284 ) ) ;
#14748 = DIRECTION ( 'NONE',  ( -0.000000000000000000, 1.000000000000000000, -0.000000000000000000 ) ) ;
#14749 = DIRECTION ( 'NONE',  ( 1.000000000000000000, 0.000000000000000000, 0.000000000000000000 ) ) ;
#14750 = PLANE ( 'NONE',  #8743 ) ;
#14751 = CARTESIAN_POINT ( 'NONE',  ( -36.03642545851251100, 84.22855780814606419, 55.00000000000001421 ) ) ;
#14752 = VERTEX_POINT ( 'NONE', #5090 ) ;
#14753 = AXIS2_PLACEMENT_3D ( 'NONE', #18322, #16907, #15502 ) ;
#14754 = EDGE_CURVE ( 'NONE', #7519, #748, #14824, .T. ) ;
#14755 = EDGE_CURVE ( 'NONE', #2330, #299, #1530, .T. ) ;
#14756 = CIRCLE ( 'NONE', #3724, 7.500000000000000000 ) ;
#14757 = EDGE_CURVE ( 'NONE', #15598, #14963, #6491, .T. ) ;
#14758 = AXIS2_PLACEMENT_3D ( 'NONE', #11894, #9371, #15069 ) ;
#14759 = DIRECTION ( 'NONE',  ( 0.000000000000000000, -1.000000000000000000, 1.181335735494911869E-16 ) ) ;
#14760 = ORIENTED_EDGE ( 'NONE', *, *, #14754, .F. ) ;
#14761 = ADVANCED_FACE ( 'NONE', ( #9494 ), #17627, .T. ) ;
#14762 = FACE_OUTER_BOUND ( 'NONE', #8160, .T. ) ;
#14763 = PRESENTATION_STYLE_ASSIGNMENT (( #11867 ) ) ;
#14764 = ORIENTED_EDGE ( 'NONE', *, *, #14604, .F. ) ;
#14765 = EDGE_LOOP ( 'NONE', ( #12584, #7747, #6566, #7294 ) ) ;
#14766 = AXIS2_PLACEMENT_3D ( 'NONE', #1927, #7637, #13706 ) ;
#14767 = ORIENTED_EDGE ( 'NONE', *, *, #10999, .T. ) ;
#14768 = CONICAL_SURFACE ( 'NONE', #15691, 7.500000000000007105, 0.1302312384721128480 ) ;
#14769 = EDGE_CURVE ( 'NONE', #15127, #2177, #10808, .T. ) ;
#14770 = CIRCLE ( 'NONE', #18379, 4.599999999999992539 ) ;
#14771 = LINE ( 'NONE', #750, #737 ) ;
#14772 = CARTESIAN_POINT ( 'NONE',  ( -57.08002265617300708, 84.22855780814606419, -28.00000000000000355 ) ) ;
#14773 = EDGE_CURVE ( 'NONE', #11278, #15985, #10915, .T. ) ;
#14774 = LINE ( 'NONE', #7751, #1032 ) ;
#14775 = LINE ( 'NONE', #4405, #14358 ) ;
#14776 = CARTESIAN_POINT ( 'NONE',  ( -71.24615306438070661, 141.0590213152292449, 15.00000000000006928 ) ) ;
#14777 = CYLINDRICAL_SURFACE ( 'NONE', #5726, 4.600000000000006750 ) ;
#14778 = ORIENTED_EDGE ( 'NONE', *, *, #150, .T. ) ;
#14779 = CARTESIAN_POINT ( 'NONE',  ( -71.24615306438067819, 145.0894847045637732, -15.00000000000001421 ) ) ;
#14780 = CARTESIAN_POINT ( 'NONE',  ( -75.72335493167710752, 61.53592931583062864, -28.00000000000000355 ) ) ;
#14781 = CARTESIAN_POINT ( 'NONE',  ( -62.30871503255384170, 95.58244595420320877, -15.00000000000001421 ) ) ;
#14782 = ORIENTED_EDGE ( 'NONE', *, *, #7352, .F. ) ;
#14783 = CIRCLE ( 'NONE', #16890, 40.40389983439752086 ) ;
#14784 = FACE_OUTER_BOUND ( 'NONE', #7892, .T. ) ;
#14785 = CIRCLE ( 'NONE', #5817, 12.49999999999999112 ) ;
#14786 = DIRECTION ( 'NONE',  ( 1.000000000000000000, 0.000000000000000000, 3.771137991253923150E-16 ) ) ;
#14788 = ORIENTED_EDGE ( 'NONE', *, *, #11176, .T. ) ;
#14787 = VECTOR ( 'NONE', #11136, 1000.000000000000114 ) ;
#14789 = ORIENTED_EDGE ( 'NONE', *, *, #18306, .T. ) ;
#14790 = EDGE_CURVE ( 'NONE', #13337, #7261, #3912, .T. ) ;
#14791 = CARTESIAN_POINT ( 'NONE',  ( -71.24615306438076345, 122.2094654152292037, -167.1454815528550739 ) ) ;
#14792 = CARTESIAN_POINT ( 'NONE',  ( -71.24615306438063556, 138.8062994045637595, 15.00000000000006928 ) ) ;
#14793 = CARTESIAN_POINT ( 'NONE',  ( -56.59294758719027385, 94.46597735006069740, 15.00000000000006928 ) ) ;
#14794 = VERTEX_POINT ( 'NONE', #8087 ) ;
#14795 = VECTOR ( 'NONE', #16246, 1000.000000000000000 ) ;
#14796 = AXIS2_PLACEMENT_3D ( 'NONE', #10825, #5107, #9429 ) ;
#14797 = CARTESIAN_POINT ( 'NONE',  ( 84.41679105416972106, 84.22855780814606419, 62.50000000000001421 ) ) ;
#14798 = ORIENTED_EDGE ( 'NONE', *, *, #1933, .F. ) ;
#14799 = CARTESIAN_POINT ( 'NONE',  ( -57.08002265617300708, 84.22855780814606419, -167.1454815528550739 ) ) ;
#14800 = CYLINDRICAL_SURFACE ( 'NONE', #11419, 4.600000000000006750 ) ;
#14801 = CARTESIAN_POINT ( 'NONE',  ( -77.86238486193855124, 87.56553636334633950, 55.76536848324052897 ) ) ;
#14802 = DIRECTION ( 'NONE',  ( -0.000000000000000000, -1.000000000000000000, -0.000000000000000000 ) ) ;
#14803 = ORIENTED_EDGE ( 'NONE', *, *, #11245, .T. ) ;
#14804 = CARTESIAN_POINT ( 'NONE',  ( -57.08002265617300708, 84.22855780814606419, 68.73600986863397111 ) ) ;
#14805 = ORIENTED_EDGE ( 'NONE', *, *, #11687, .T. ) ;
#14806 = FACE_OUTER_BOUND ( 'NONE', #193, .T. ) ;
#14807 = VERTEX_POINT ( 'NONE', #12316 ) ;
#14808 = EDGE_CURVE ( 'NONE', #10723, #646, #16318, .T. ) ;
#14809 = ORIENTED_EDGE ( 'NONE', *, *, #8599, .T. ) ;
#14810 =( REPRESENTATION_RELATIONSHIP ('NONE','NONE', #359, #15047 ) REPRESENTATION_RELATIONSHIP_WITH_TRANSFORMATION ( #17155 )SHAPE_REPRESENTATION_RELATIONSHIP( ) );
#14811 = ORIENTED_EDGE ( 'NONE', *, *, #14967, .T. ) ;
#14812 = EDGE_CURVE ( 'NONE', #5095, #3710, #8975, .T. ) ;
#14813 = CARTESIAN_POINT ( 'NONE',  ( -68.99615306438070661, 115.1073470881302256, 15.00000000000006928 ) ) ;
#14814 = EDGE_LOOP ( 'NONE', ( #1998, #1517, #16483, #4349 ) ) ;
#14815 = FACE_OUTER_BOUND ( 'NONE', #8451, .T. ) ;
#14816 = CARTESIAN_POINT ( 'NONE',  ( -47.80867013224673912, 89.78028827820993740, 15.00000000000006928 ) ) ;
#14817 = ORIENTED_EDGE ( 'NONE', *, *, #6991, .F. ) ;
#14818 = DIRECTION ( 'NONE',  ( -5.204170427930409450E-16, 0.000000000000000000, 1.000000000000000000 ) ) ;
#14819 = ORIENTED_EDGE ( 'NONE', *, *, #12965, .T. ) ;
#14820 = CARTESIAN_POINT ( 'NONE',  ( -68.99615306438089135, 79.93497208166267853, 15.00000000000006928 ) ) ;
#14821 = DIRECTION ( 'NONE',  ( -2.062304371594500494E-16, 1.000000000000000000, 0.000000000000000000 ) ) ;
#14822 = ORIENTED_EDGE ( 'NONE', *, *, #14312, .F. ) ;
#14823 = CARTESIAN_POINT ( 'NONE',  ( 0.000000000000000000, 0.000000000000000000, 0.000000000000000000 ) ) ;
#14824 = LINE ( 'NONE', #4996, #5659 ) ;
#14825 = ORIENTED_EDGE ( 'NONE', *, *, #14871, .T. ) ;
#14826 = EDGE_CURVE ( 'NONE', #14359, #10700, #10710, .T. ) ;
#14827 = ORIENTED_EDGE ( 'NONE', *, *, #11507, .F. ) ;
#14828 = FACE_OUTER_BOUND ( 'NONE', #3029, .T. ) ;
#14829 = FACE_OUTER_BOUND ( 'NONE', #6833, .T. ) ;
#14830 = VERTEX_POINT ( 'NONE', #6303 ) ;
#14831 = ADVANCED_FACE ( 'NONE', ( #3506 ), #14909, .F. ) ;
#14832 = CARTESIAN_POINT ( 'NONE',  ( 0.000000000000000000, 0.000000000000000000, 0.000000000000000000 ) ) ;
#14833 =( LENGTH_UNIT ( ) NAMED_UNIT ( * ) SI_UNIT ( .MILLI., .METRE. ) );
#14834 = CARTESIAN_POINT ( 'NONE',  ( -71.24615306438100504, 53.09442711522921599, -167.1454815528550739 ) ) ;
#14835 = DIRECTION ( 'NONE',  ( 0.000000000000000000, 0.000000000000000000, 1.000000000000000000 ) ) ;
#14836 = ORIENTED_EDGE ( 'NONE', *, *, #10179, .F. ) ;
#14837 = CARTESIAN_POINT ( 'NONE',  ( -71.24615306438106188, 34.24487121522926003, -15.00000000000001421 ) ) ;
#14838 = CARTESIAN_POINT ( 'NONE',  ( -68.99615306438097662, 61.08541618166268705, -167.1454815528550739 ) ) ;
#14839 = DIRECTION ( 'NONE',  ( 1.156482317317869999E-16, 0.000000000000000000, 1.000000000000000000 ) ) ;
#14840 = CYLINDRICAL_SURFACE ( 'NONE', #12029, 180.8515291679561585 ) ;
#14841 = DIRECTION ( 'NONE',  ( 4.029365176583844474E-15, 0.000000000000000000, -1.000000000000000000 ) ) ;
#14842 = VERTEX_POINT ( 'NONE', #13529 ) ;
#14843 = LINE ( 'NONE', #6227, #736 ) ;
#14844 = DIRECTION ( 'NONE',  ( 0.9396926207859084279, 0.3420201433256686574, 4.890320548438448905E-16 ) ) ;
#14845 = EDGE_CURVE ( 'NONE', #16693, #9789, #714, .T. ) ;
#14846 = ORIENTED_EDGE ( 'NONE', *, *, #2182, .T. ) ;
#14847 = EDGE_CURVE ( 'NONE', #4088, #16289, #2358, .T. ) ;
#14848 = FACE_OUTER_BOUND ( 'NONE', #5482, .T. ) ;
#14849 = DIRECTION ( 'NONE',  ( -1.000000000000000000, 0.000000000000000000, 0.000000000000000000 ) ) ;
#14850 = ORIENTED_EDGE ( 'NONE', *, *, #13981, .T. ) ;
#14851 = ORIENTED_EDGE ( 'NONE', *, *, #5626, .F. ) ;
#14852 = FACE_OUTER_BOUND ( 'NONE', #3323, .T. ) ;
#14853 = EDGE_CURVE ( 'NONE', #15127, #5660, #2683, .T. ) ;
#14854 = ORIENTED_EDGE ( 'NONE', *, *, #16113, .T. ) ;
#14855 = EDGE_CURVE ( 'NONE', #9751, #10505, #14008, .T. ) ;
#14856 = CARTESIAN_POINT ( 'NONE',  ( 124.5381772159375942, -46.83756720124470263, 57.00000000000000000 ) ) ;
#14857 = FACE_OUTER_BOUND ( 'NONE', #18106, .T. ) ;
#14858 = LINE ( 'NONE', #9079, #5798 ) ;
#14859 = PLANE ( 'NONE',  #2704 ) ;
#14860 = LINE ( 'NONE', #5037, #16876 ) ;
#14861 = CYLINDRICAL_SURFACE ( 'NONE', #1262, 4.600000000000013856 ) ;
#14862 = EDGE_LOOP ( 'NONE', ( #8434, #14410, #11650, #6505 ) ) ;
#14863 = EDGE_CURVE ( 'NONE', #15269, #14752, #13426, .T. ) ;
#14864 = DIRECTION ( 'NONE',  ( -1.000000000000000000, -0.000000000000000000, -0.000000000000000000 ) ) ;
#14865 = CARTESIAN_POINT ( 'NONE',  ( -76.14500017491396022, 61.88899956654809387, -26.29040544024000425 ) ) ;
#14866 = PLANE ( 'NONE',  #2701 ) ;
#14867 = EDGE_CURVE ( 'NONE', #16085, #16195, #3803, .T. ) ;
#14868 = ORIENTED_EDGE ( 'NONE', *, *, #5364, .T. ) ;
#14869 = DIRECTION ( 'NONE',  ( 0.000000000000000000, 0.000000000000000000, 1.000000000000000000 ) ) ;
#14870 = CARTESIAN_POINT ( 'NONE',  ( -68.99615306438067819, 142.7668250816626596, 15.00000000000006928 ) ) ;
#14871 = EDGE_CURVE ( 'NONE', #13777, #12432, #14105, .T. ) ;
#14872 = VERTEX_POINT ( 'NONE', #15301 ) ;
#14873 = EDGE_CURVE ( 'NONE', #10224, #9544, #5485, .T. ) ;
#14874 = VECTOR ( 'NONE', #6185, 1000.000000000000000 ) ;
#14875 = EDGE_LOOP ( 'NONE', ( #12076, #11323, #8630, #16662 ) ) ;
#14876 = UNCERTAINTY_MEASURE_WITH_UNIT (LENGTH_MEASURE( 1.000000000000000082E-05 ), #3998, 'distance_accuracy_value', 'NONE');
#14877 = ADVANCED_FACE ( 'NONE', ( #9598 ), #11013, .T. ) ;
#14878 = CYLINDRICAL_SURFACE ( 'NONE', #9075, 172.7605492041889477 ) ;
#14879 = DIRECTION ( 'NONE',  ( -1.000000000000000000, 6.033820786006295184E-15, 0.000000000000000000 ) ) ;
#14880 = DIRECTION ( 'NONE',  ( -0.9396926207859084279, 0.3420201433256686574, -4.890320548438448905E-16 ) ) ;
#14881 = DIRECTION ( 'NONE',  ( 0.9396926207859069846, 0.3420201433256723766, 0.000000000000000000 ) ) ;
#14882 = ORIENTED_EDGE ( 'NONE', *, *, #10634, .F. ) ;
#14883 = CARTESIAN_POINT ( 'NONE',  ( -107.5676225674731654, 57.88796029049330372, -26.35917033480641436 ) ) ;
#14884 = CARTESIAN_POINT ( 'NONE',  ( -71.24615306438091977, 75.08557566522922855, 15.00000000000006928 ) ) ;
#14885 = VERTEX_POINT ( 'NONE', #8495 ) ;
#14886 = VECTOR ( 'NONE', #10858, 1000.000000000000000 ) ;
#14887 = DIRECTION ( 'NONE',  ( 1.000000000000000000, 0.000000000000000000, 0.000000000000000000 ) ) ;
#14888 = DIRECTION ( 'NONE',  ( -1.000000000000000000, -3.016910393003147592E-15, 0.000000000000000000 ) ) ;
#14889 = DIRECTION ( 'NONE',  ( 0.000000000000000000, 0.000000000000000000, 1.000000000000000000 ) ) ;
#14890 = CARTESIAN_POINT ( 'NONE',  ( -114.8884567811963677, -93.39009998357855125, 6.425136209963392631 ) ) ;
#14891 = ORIENTED_EDGE ( 'NONE', *, *, #16480, .T. ) ;
#14892 = DIRECTION ( 'NONE',  ( 1.000000000000000000, 0.000000000000000000, 0.000000000000000000 ) ) ;
#14893 = ORIENTED_EDGE ( 'NONE', *, *, #7820, .F. ) ;
#14894 = CARTESIAN_POINT ( 'NONE',  ( -68.99615306438070661, 130.8153103381302742, -15.00000000000001421 ) ) ;
#14895 = ORIENTED_EDGE ( 'NONE', *, *, #8712, .F. ) ;
#14896 = AXIS2_PLACEMENT_3D ( 'NONE', #12938, #18460, #7130 ) ;
#14897 = ORIENTED_EDGE ( 'NONE', *, *, #17156, .T. ) ;
#14898 = EDGE_LOOP ( 'NONE', ( #14122, #12202, #564, #3713 ) ) ;
#14899 = DIRECTION ( 'NONE',  ( -1.000000000000000000, 0.000000000000000000, -1.110223024625157172E-14 ) ) ;
#14900 = DIRECTION ( 'NONE',  ( 1.047634945911799279E-14, -0.000000000000000000, -1.000000000000000000 ) ) ;
#14901 = ORIENTED_EDGE ( 'NONE', *, *, #10429, .T. ) ;
#14902 = DIRECTION ( 'NONE',  ( -1.000000000000000000, 0.000000000000000000, 0.000000000000000000 ) ) ;
#14903 = VERTEX_POINT ( 'NONE', #1291 ) ;
#14904 = CIRCLE ( 'NONE', #17305, 3.999999999999989786 ) ;
#14905 = SPHERICAL_SURFACE ( 'NONE', #655, 17.12963335357822103 ) ;
#14906 = DIRECTION ( 'NONE',  ( -1.000000000000000000, 0.000000000000000000, 0.000000000000000000 ) ) ;
#14907 = AXIS2_PLACEMENT_3D ( 'NONE', #1729, #15698, #18495 ) ;
#14908 = CARTESIAN_POINT ( 'NONE',  ( -57.08002265617300708, 84.22855780814606419, 15.00000000000006928 ) ) ;
#14909 = CYLINDRICAL_SURFACE ( 'NONE', #1809, 3.999999999999989786 ) ;
#14910 = ORIENTED_EDGE ( 'NONE', *, *, #9022, .F. ) ;
#14911 = VERTEX_POINT ( 'NONE', #18312 ) ;
#14912 = VECTOR ( 'NONE', #1782, 1000.000000000000227 ) ;
#14913 = CARTESIAN_POINT ( 'NONE',  ( -68.99615306438089135, 67.36860148166267948, 15.00000000000006928 ) ) ;
#14914 = CARTESIAN_POINT ( 'NONE',  ( -63.37199650155329778, 75.44273092821040905, 15.00000000000006928 ) ) ;
#14915 = VERTEX_POINT ( 'NONE', #8296 ) ;
#14916 = VECTOR ( 'NONE', #1873, 1000.000000000000000 ) ;
#14917 = CYLINDRICAL_SURFACE ( 'NONE', #5832, 12.50000000000000355 ) ;
#14918 =( NAMED_UNIT ( * ) SI_UNIT ( $, .STERADIAN. ) SOLID_ANGLE_UNIT ( ) );
#14919 = DIRECTION ( 'NONE',  ( -1.000000000000000000, -3.774758283725530975E-14, 1.387778780781445182E-16 ) ) ;
#14920 = FACE_OUTER_BOUND ( 'NONE', #6371, .T. ) ;
#14921 = ORIENTED_EDGE ( 'NONE', *, *, #12610, .F. ) ;
#14922 = LINE ( 'NONE', #17642, #17931 ) ;
#14923 = DIRECTION ( 'NONE',  ( 0.9396926207859084279, 0.3420201433256686574, -1.086737899652989892E-16 ) ) ;
#14924 = LINE ( 'NONE', #8967, #12742 ) ;
#14925 = DIRECTION ( 'NONE',  ( -5.204170427930409450E-16, 0.000000000000000000, 1.000000000000000000 ) ) ;
#14926 = ORIENTED_EDGE ( 'NONE', *, *, #6778, .F. ) ;
#14927 = CARTESIAN_POINT ( 'NONE',  ( -71.24615306438063556, 141.9478920545637948, 15.00000000000006928 ) ) ;
#14928 = FACE_OUTER_BOUND ( 'NONE', #1753, .T. ) ;
#14929 = EDGE_LOOP ( 'NONE', ( #7771, #17167, #4769, #13935, #15494 ) ) ;
#14930 = EDGE_CURVE ( 'NONE', #6388, #11390, #6585, .T. ) ;
#14931 = FACE_OUTER_BOUND ( 'NONE', #4720, .T. ) ;
#14932 = AXIS2_PLACEMENT_3D ( 'NONE', #3009, #7395, #6240 ) ;
#14933 = CARTESIAN_POINT ( 'NONE',  ( 5.299999999999998934, 7.505553499465141165, -1.387778780781445676E-14 ) ) ;
#14934 = VERTEX_POINT ( 'NONE', #15412 ) ;
#14935 = ORIENTED_EDGE ( 'NONE', *, *, #12737, .T. ) ;
#14936 = B_SPLINE_CURVE_WITH_KNOTS ( 'NONE', 3,
 ( #9349, #16539, #9530, #15046, #929, #16720, #13745, #3919, #15233, #2240, #10949, #18045, #2521, #18238 ),
 .UNSPECIFIED., .F., .F.,
 ( 4, 2, 2, 2, 2, 2, 4 ),
 ( 0.01646133141517134441, 0.01782527105796415101, 0.01918921070075695762, 0.01987118052215335745, 0.02021216543285155390, 0.02055315034354975381, 0.02191708998634258124 ),
 .UNSPECIFIED. ) ;
#14937 = LINE ( 'NONE', #10661, #9359 ) ;
#14938 = AXIS2_PLACEMENT_3D ( 'NONE', #12446, #18138, #13934 ) ;
#14939 = ORIENTED_EDGE ( 'NONE', *, *, #2655, .T. ) ;
#14940 = PLANE ( 'NONE',  #3725 ) ;
#14941 = FACE_OUTER_BOUND ( 'NONE', #10689, .T. ) ;
#14943 = EDGE_CURVE ( 'NONE', #6219, #10428, #1191, .T. ) ;
#14942 = AXIS2_PLACEMENT_3D ( 'NONE', #12732, #9719, #15425 ) ;
#14944 = LINE ( 'NONE', #2141, #9094 ) ;
#14945 = ADVANCED_FACE ( 'NONE', ( #2494 ), #5201, .F. ) ;
#14946 = DIRECTION ( 'NONE',  ( -0.9396926207859084279, 0.3420201433256686574, 1.086737899652989892E-16 ) ) ;
#14947 = CIRCLE ( 'NONE', #15559, 12.58237727243326987 ) ;
#14948 = DIRECTION ( 'NONE',  ( 1.000000000000000000, 0.000000000000000000, 0.000000000000000000 ) ) ;
#14949 = DIRECTION ( 'NONE',  ( 0.9396926207859084279, 0.3420201433256686574, -1.086737899652989892E-16 ) ) ;
#14950 = ORIENTED_EDGE ( 'NONE', *, *, #15877, .T. ) ;
#14951 = CARTESIAN_POINT ( 'NONE',  ( -76.06859087019410026, 61.82386385984740684, -25.61244817148770991 ) ) ;
#14952 = CARTESIAN_POINT ( 'NONE',  ( -57.08002265617300708, 84.22855780814606419, 35.00000000000000000 ) ) ;
#14953 = ORIENTED_EDGE ( 'NONE', *, *, #9596, .T. ) ;
#14954 = EDGE_CURVE ( 'NONE', #15261, #768, #8095, .T. ) ;
#14955 = CIRCLE ( 'NONE', #3028, 10.24900000000000055 ) ;
#14956 = EDGE_CURVE ( 'NONE', #17628, #5348, #10925, .T. ) ;
#14957 = CARTESIAN_POINT ( 'NONE',  ( -31.74593505105995916, -91.08423613455721579, -10.65431531532567710 ) ) ;
#14958 = DIRECTION ( 'NONE',  ( 1.000000000000000000, 0.000000000000000000, 0.000000000000000000 ) ) ;
#14959 = VERTEX_POINT ( 'NONE', #16610 ) ;
#14960 = EDGE_CURVE ( 'NONE', #5095, #7404, #13917, .T. ) ;
#14961 = AXIS2_PLACEMENT_3D ( 'NONE', #11188, #9684, #16597 ) ;
#14962 = VECTOR ( 'NONE', #17063, 1000.000000000000000 ) ;
#14963 = VERTEX_POINT ( 'NONE', #3989 ) ;
#14964 = EDGE_CURVE ( 'NONE', #8931, #12366, #13814, .T. ) ;
#14965 = CARTESIAN_POINT ( 'NONE',  ( -65.18918009136292824, 57.88796029049328240, 26.35917033480641436 ) ) ;
#14966 = CARTESIAN_POINT ( 'NONE',  ( -57.08002265617300708, 84.22855780814606419, 15.00000000000006928 ) ) ;
#14967 = EDGE_CURVE ( 'NONE', #4389, #9420, #9704, .T. ) ;
#14968 = CYLINDRICAL_SURFACE ( 'NONE', #10005, 10.24900000000000766 ) ;
#14969 = DIRECTION ( 'NONE',  ( 0.000000000000000000, 1.000000000000000000, 0.000000000000000000 ) ) ;
#14970 = EDGE_CURVE ( 'NONE', #3203, #3299, #12716, .T. ) ;
#14971 = ORIENTED_EDGE ( 'NONE', *, *, #16960, .F. ) ;
#14972 = AXIS2_PLACEMENT_3D ( 'NONE', #10971, #8054, #3850 ) ;
#14973 = EDGE_CURVE ( 'NONE', #15423, #7166, #11300, .T. ) ;
#14974 = ORIENTED_EDGE ( 'NONE', *, *, #13163, .F. ) ;
#14975 = CARTESIAN_POINT ( 'NONE',  ( -66.40868851600848188, 112.0764521540501875, 25.00000000000000355 ) ) ;
#14976 = LINE ( 'NONE', #9197, #3321 ) ;
#14977 = DIRECTION ( 'NONE',  ( 0.000000000000000000, 0.000000000000000000, 1.000000000000000000 ) ) ;
#14978 = FACE_OUTER_BOUND ( 'NONE', #17044, .T. ) ;
#14979 = CIRCLE ( 'NONE', #17660, 3.999999999999989786 ) ;
#14980 = VECTOR ( 'NONE', #10117, 1000.000000000000000 ) ;
#14981 = VERTEX_POINT ( 'NONE', #7262 ) ;
#14982 = DIRECTION ( 'NONE',  ( 0.000000000000000000, 0.000000000000000000, 1.000000000000000000 ) ) ;
#14983 = ORIENTED_EDGE ( 'NONE', *, *, #3198, .T. ) ;
#14984 = EDGE_CURVE ( 'NONE', #9065, #13724, #17688, .T. ) ;
#14985 = ADVANCED_FACE ( 'NONE', ( #17256 ), #237, .T. ) ;
#14986 = EDGE_CURVE ( 'NONE', #17238, #7705, #12985, .T. ) ;
#14987 = FACE_OUTER_BOUND ( 'NONE', #5688, .T. ) ;
#14988 = VERTEX_POINT ( 'NONE', #61 ) ;
#14989 = AXIS2_PLACEMENT_3D ( 'NONE', #696, #7624, #7979 ) ;
#14990 = ORIENTED_EDGE ( 'NONE', *, *, #972, .T. ) ;
#14991 = VECTOR ( 'NONE', #12993, 1000.000000000000000 ) ;
#14992 = VECTOR ( 'NONE', #6826, 1000.000000000000000 ) ;
#14993 = CARTESIAN_POINT ( 'NONE',  ( -92.59262256747319952, 57.88796029049329661, 30.35917033480640370 ) ) ;
#14994 = ORIENTED_EDGE ( 'NONE', *, *, #4129, .F. ) ;
#14995 = ADVANCED_FACE ( 'NONE', ( #4366 ), #10072, .T. ) ;
#14996 = CARTESIAN_POINT ( 'NONE',  ( -67.59262256747319952, 110.5691553257988460, 26.35917033480641436 ) ) ;
#14997 = EDGE_CURVE ( 'NONE', #7762, #9243, #592, .T. ) ;
#14998 = PLANE ( 'NONE',  #15063 ) ;
#14999 = ORIENTED_EDGE ( 'NONE', *, *, #10856, .F. ) ;
#15000 = AXIS2_PLACEMENT_3D ( 'NONE', #875, #17611, #17804 ) ;
#15001 = LINE ( 'NONE', #16216, #1816 ) ;
#15002 = ORIENTED_EDGE ( 'NONE', *, *, #1162, .T. ) ;
#15003 = DIRECTION ( 'NONE',  ( -1.000000000000000000, 0.000000000000000000, 1.387778780781446662E-16 ) ) ;
#15004 = DIRECTION ( 'NONE',  ( 0.000000000000000000, -0.000000000000000000, 1.000000000000000000 ) ) ;
#15005 = ORIENTED_EDGE ( 'NONE', *, *, #6165, .F. ) ;
#15006 = CIRCLE ( 'NONE', #11160, 40.40389983439752086 ) ;
#15007 = CIRCLE ( 'NONE', #83, 4.599999999999999645 ) ;
#15008 = DIRECTION ( 'NONE',  ( 0.000000000000000000, 1.000000000000000000, 0.000000000000000000 ) ) ;
#15009 = CARTESIAN_POINT ( 'NONE',  ( -70.71978124295696944, -91.08423613455721579, 5.204170427930421283E-15 ) ) ;
#15010 = ORIENTED_EDGE ( 'NONE', *, *, #105, .T. ) ;
#15011 = ORIENTED_EDGE ( 'NONE', *, *, #47, .F. ) ;
#15012 = VECTOR ( 'NONE', #6216, 1000.000000000000000 ) ;
#15013 = ORIENTED_EDGE ( 'NONE', *, *, #8810, .T. ) ;
#15014 = DIRECTION ( 'NONE',  ( 0.9396926207859097602, 0.3420201433256649381, 4.890320548438455808E-16 ) ) ;
#15015 = CARTESIAN_POINT ( 'NONE',  ( -78.12361985383350316, 84.22855780814606419, -62.50000000000000000 ) ) ;
#15016 = ORIENTED_EDGE ( 'NONE', *, *, #3302, .F. ) ;
#15017 = AXIS2_PLACEMENT_3D ( 'NONE', #18147, #1214, #14129 ) ;
#15018 = VECTOR ( 'NONE', #4327, 1000.000000000000000 ) ;
#15019 = DIRECTION ( 'NONE',  ( 0.000000000000000000, 0.000000000000000000, -1.000000000000000000 ) ) ;
#15021 = VECTOR ( 'NONE', #5868, 1000.000000000000000 ) ;
#15020 = CARTESIAN_POINT ( 'NONE',  ( -76.74163717699387632, 76.72829797731421309, 62.01011918307220583 ) ) ;
#15022 = CARTESIAN_POINT ( 'NONE',  ( -71.24615306438076345, 131.6342433652292243, -167.1454815528550739 ) ) ;
#15023 = CARTESIAN_POINT ( 'NONE',  ( 276.3098885457529832, -32.62665103886256190, 7.000000000000010658 ) ) ;
#15024 = ORIENTED_EDGE ( 'NONE', *, *, #13167, .T. ) ;
#15025 = LINE ( 'NONE', #9329, #2111 ) ;
#15026 = CARTESIAN_POINT ( 'NONE',  ( -68.99615306438100504, 42.23586028166270978, -167.1454815528550739 ) ) ;
#15027 = SURFACE_SIDE_STYLE ('',( #16617 ) ) ;
#15028 = CARTESIAN_POINT ( 'NONE',  ( -28.94822502443852841, 53.44157543122878451, 24.93952570249303946 ) ) ;
#15029 = EDGE_LOOP ( 'NONE', ( #876, #3003, #12587, #11639 ) ) ;
#15030 = DIRECTION ( 'NONE',  ( 0.000000000000000000, 0.000000000000000000, 1.000000000000000000 ) ) ;
#15031 = CARTESIAN_POINT ( 'NONE',  ( -68.99615306438100504, 48.51904558166270220, 15.00000000000006928 ) ) ;
#15032 = VERTEX_POINT ( 'NONE', #8857 ) ;
#15033 =( GEOMETRIC_REPRESENTATION_CONTEXT ( 3 ) GLOBAL_UNCERTAINTY_ASSIGNED_CONTEXT ( ( #15452 ) ) GLOBAL_UNIT_ASSIGNED_CONTEXT ( ( #4462, #3067, #11589 ) ) REPRESENTATION_CONTEXT ( 'NONE', 'WORKASPACE' ) );
#15034 = DIRECTION ( 'NONE',  ( 0.3420201433256635504, 0.9396926207859103153, -0.000000000000000000 ) ) ;
#15035 = VECTOR ( 'NONE', #5032, 1000.000000000000227 ) ;
#15036 = CARTESIAN_POINT ( 'NONE',  ( -36.53934929799278564, 79.65130292775349119, 56.55370057778164750 ) ) ;
#15037 = ORIENTED_EDGE ( 'NONE', *, *, #3103, .F. ) ;
#15038 = AXIS2_PLACEMENT_3D ( 'NONE', #874, #4703, #16111 ) ;
#15039 = EDGE_CURVE ( 'NONE', #583, #12181, #14345, .T. ) ;
#15040 = ORIENTED_EDGE ( 'NONE', *, *, #4574, .T. ) ;
#15041 = DIRECTION ( 'NONE',  ( 0.3420201433256687684, 0.9396926207859084279, -0.000000000000000000 ) ) ;
#15042 = CLOSED_SHELL ( 'NONE', ( #14718, #7662, #1834, #13950, #1810, #2663, #13443, #7566, #14210, #11780, #17701, #10417, #126, #12016 ) ) ;
#15043 = ORIENTED_EDGE ( 'NONE', *, *, #11958, .T. ) ;
#15044 = DIRECTION ( 'NONE',  ( -5.204170427930409450E-16, 0.000000000000000000, 1.000000000000000000 ) ) ;
#15045 = LINE ( 'NONE', #8027, #17704 ) ;
#15046 = CARTESIAN_POINT ( 'NONE',  ( -66.75451753366466789, 59.92410785088754466, -28.00000000000000000 ) ) ;
#15047 = SHAPE_REPRESENTATION ( 'Drive Gear', ( #16217 ), #9669 ) ;
#15048 = CARTESIAN_POINT ( 'NONE',  ( -71.24615306438070661, 141.0590213152292449, -15.00000000000001421 ) ) ;
#15049 = AXIS2_PLACEMENT_3D ( 'NONE', #3806, #3894, #18022 ) ;
#15050 = DIRECTION ( 'NONE',  ( 0.000000000000000000, -1.000000000000000000, -0.000000000000000000 ) ) ;
#15051 = CIRCLE ( 'NONE', #1618, 95.91469608272775815 ) ;
#15052 = LINE ( 'NONE', #11969, #13792 ) ;
#15053 = PRODUCT_DEFINITION_SHAPE ( 'NONE', 'NONE',  #18529 ) ;
#15054 = ORIENTED_EDGE ( 'NONE', *, *, #4698, .F. ) ;
#15055 = LINE ( 'NONE', #3361, #6347 ) ;
#15056 = CYLINDRICAL_SURFACE ( 'NONE', #12256, 11.04359719766049430 ) ;
#15057 = VERTEX_POINT ( 'NONE', #8662 ) ;
#15058 = AXIS2_PLACEMENT_3D ( 'NONE', #2466, #12862, #16869 ) ;
#15059 = CARTESIAN_POINT ( 'NONE',  ( -28.46967348631369177, -91.80659809767261947, -8.049312157728762074 ) ) ;
#15060 = FACE_OUTER_BOUND ( 'NONE', #13009, .T. ) ;
#15061 = VERTEX_POINT ( 'NONE', #14368 ) ;
#15062 = VECTOR ( 'NONE', #15030, 1000.000000000000000 ) ;
#15063 = AXIS2_PLACEMENT_3D ( 'NONE', #9576, #6293, #16309 ) ;
#15064 = VECTOR ( 'NONE', #9347, 1000.000000000000000 ) ;
#15065 = ORIENTED_EDGE ( 'NONE', *, *, #11587, .F. ) ;
#15066 = PRODUCT_DEFINITION_CONTEXT ( 'detailed design', #7176, 'design' ) ;
#15067 = CARTESIAN_POINT ( 'NONE',  ( -98.90286936182239685, -96.08423613455721579, 5.654315315325477265 ) ) ;
#15068 = CARTESIAN_POINT ( 'NONE',  ( -36.77424632280495587, 74.98691627113812785, 102.5000000000000000 ) ) ;
#15069 = DIRECTION ( 'NONE',  ( 1.000000000000000000, 0.000000000000000000, 0.000000000000000000 ) ) ;
#15070 = LINE ( 'NONE', #7871, #2157 ) ;
#15071 = EDGE_CURVE ( 'NONE', #2577, #6571, #5759, .T. ) ;
#15072 = FACE_OUTER_BOUND ( 'NONE', #12171, .T. ) ;
#15073 = CARTESIAN_POINT ( 'NONE',  ( -57.35243698450333483, 71.73152654333280509, -15.00000000000001421 ) ) ;
#15074 = VERTEX_POINT ( 'NONE', #5855 ) ;
#15075 = AXIS2_PLACEMENT_3D ( 'NONE', #8776, #1473, #8866 ) ;
#15076 = DIRECTION ( 'NONE',  ( 1.000000000000000000, 0.000000000000000000, 3.771137991253928573E-16 ) ) ;
#15077 = DIRECTION ( 'NONE',  ( 0.000000000000000000, 1.000000000000000000, -0.000000000000000000 ) ) ;
#15078 = CARTESIAN_POINT ( 'NONE',  ( -69.52933024547458274, 85.35316464920589397, 15.00000000000006750 ) ) ;
#15079 = LINE ( 'NONE', #6274, #7844 ) ;
#15080 = AXIS2_PLACEMENT_3D ( 'NONE', #11246, #16931, #17286 ) ;
#15081 = ORIENTED_EDGE ( 'NONE', *, *, #4770, .T. ) ;
#15082 = VECTOR ( 'NONE', #8026, 1000.000000000000000 ) ;
#15083 = DIRECTION ( 'NONE',  ( 0.9396926207859084279, 0.3420201433256686574, 4.890320548438448905E-16 ) ) ;
#15084 = VERTEX_POINT ( 'NONE', #11570 ) ;
#15085 = DIRECTION ( 'NONE',  ( 0.000000000000000000, 0.000000000000000000, 1.000000000000000000 ) ) ;
#15086 = EDGE_LOOP ( 'NONE', ( #1066, #18233, #13151, #3819 ) ) ;
#15087 = EDGE_CURVE ( 'NONE', #1022, #15084, #11488, .T. ) ;
#15088 = EDGE_CURVE ( 'NONE', #14649, #15284, #14551, .T. ) ;
#15089 = ORIENTED_EDGE ( 'NONE', *, *, #8250, .F. ) ;
#15090 = AXIS2_PLACEMENT_3D ( 'NONE', #2771, #992, #5289 ) ;
#15091 = PRESENTATION_LAYER_ASSIGNMENT (  '', '', ( #11822 ) ) ;
#15092 = AXIS2_PLACEMENT_3D ( 'NONE', #530, #6222, #6132 ) ;
#15093 = PRESENTATION_STYLE_ASSIGNMENT (( #15174 ) ) ;
#15094 = DIRECTION ( 'NONE',  ( -0.9396926207859097602, 0.3420201433256649381, -4.890320548438455808E-16 ) ) ;
#15095 = EDGE_CURVE ( 'NONE', #8377, #3838, #11645, .T. ) ;
#15096 = ORIENTED_EDGE ( 'NONE', *, *, #4667, .F. ) ;
#15097 = EDGE_CURVE ( 'NONE', #2613, #5742, #8762, .T. ) ;
#15098 = EDGE_CURVE ( 'NONE', #4520, #11983, #7360, .T. ) ;
#15099 = DIRECTION ( 'NONE',  ( 0.000000000000000000, 1.000000000000000000, 0.000000000000000000 ) ) ;
#15100 = CARTESIAN_POINT ( 'NONE',  ( -68.99615306438077766, 111.9657544381302330, 15.00000000000006928 ) ) ;
#15101 = VERTEX_POINT ( 'NONE', #574 ) ;
#15102 = DIRECTION ( 'NONE',  ( 0.000000000000000000, 0.000000000000000000, 1.000000000000000000 ) ) ;
#15103 = EDGE_CURVE ( 'NONE', #5567, #5776, #12861, .T. ) ;
#15104 = DIRECTION ( 'NONE',  ( -2.062304371594500494E-16, 1.000000000000000000, -0.000000000000000000 ) ) ;
#15105 = ORIENTED_EDGE ( 'NONE', *, *, #1852, .T. ) ;
#15106 = LINE ( 'NONE', #5468, #5946 ) ;
#15107 = DIRECTION ( 'NONE',  ( 1.156482317317869999E-16, 0.000000000000000000, 1.000000000000000000 ) ) ;
#15108 = EDGE_CURVE ( 'NONE', #5840, #3816, #16290, .T. ) ;
#15109 = DIRECTION ( 'NONE',  ( -1.000000000000000000, -0.000000000000000000, -0.000000000000000000 ) ) ;
#15110 = DIRECTION ( 'NONE',  ( 0.000000000000000000, 0.000000000000000000, 1.000000000000000000 ) ) ;
#15111 = ORIENTED_EDGE ( 'NONE', *, *, #342, .F. ) ;
#15112 = ADVANCED_FACE ( 'NONE', ( #7087 ), #8581, .T. ) ;
#15113 = ADVANCED_FACE ( 'NONE', ( #9989 ), #11939, .F. ) ;
#15114 = ORIENTED_EDGE ( 'NONE', *, *, #8066, .T. ) ;
#15115 = FACE_OUTER_BOUND ( 'NONE', #14647, .T. ) ;
#15116 = DIRECTION ( 'NONE',  ( 0.000000000000000000, 0.000000000000000000, 1.000000000000000000 ) ) ;
#15117 = ADVANCED_FACE ( 'NONE', ( #13871 ), #14622, .T. ) ;
#15118 = ORIENTED_EDGE ( 'NONE', *, *, #14438, .T. ) ;
#15119 = CARTESIAN_POINT ( 'NONE',  ( -77.48836037079389882, 79.09395985567564935, 67.97217490261259343 ) ) ;
#15120 = CARTESIAN_POINT ( 'NONE',  ( -5.756396797216070560, 18.89541522413301067, 44.01604086321188447 ) ) ;
#15121 = DIRECTION ( 'NONE',  ( -1.000000000000000000, -0.000000000000000000, -0.000000000000000000 ) ) ;
#15122 = VERTEX_POINT ( 'NONE', #8050 ) ;
#15123 = DIRECTION ( 'NONE',  ( -0.000000000000000000, 1.000000000000000000, -0.000000000000000000 ) ) ;
#15124 = LINE ( 'NONE', #1010, #15407 ) ;
#15125 = CARTESIAN_POINT ( 'NONE',  ( -47.27059076829218043, 81.25920652595885940, -167.1454815528550739 ) ) ;
#15126 = CARTESIAN_POINT ( 'NONE',  ( -70.85175816390371040, -141.5628872026273086, -57.00000000000000000 ) ) ;
#15127 = VERTEX_POINT ( 'NONE', #16564 ) ;
#15128 = LINE ( 'NONE', #3617, #6387 ) ;
#15129 = CARTESIAN_POINT ( 'NONE',  ( -68.99615306438094819, 55.41708673813027985, -167.1454815528550739 ) ) ;
#15130 = VERTEX_POINT ( 'NONE', #9282 ) ;
#15131 = DIRECTION ( 'NONE',  ( 1.000000000000000000, 2.062304371594500494E-16, -2.775557561562890858E-16 ) ) ;
#15132 = CARTESIAN_POINT ( 'NONE',  ( -37.39948222528091293, 76.77737988954068271, 61.51276167392764194 ) ) ;
#15133 = ORIENTED_EDGE ( 'NONE', *, *, #9981, .T. ) ;
#15134 = ORIENTED_EDGE ( 'NONE', *, *, #3879, .F. ) ;
#15135 = CARTESIAN_POINT ( 'NONE',  ( -68.99615306438089135, 67.36860148166267948, 15.00000000000006928 ) ) ;
#15136 = EDGE_LOOP ( 'NONE', ( #9972, #11113, #13335, #11361 ) ) ;
#15137 = DIRECTION ( 'NONE',  ( -5.204170427930409450E-16, 0.000000000000000000, 1.000000000000000000 ) ) ;
#15138 = PLANE ( 'NONE',  #6977 ) ;
#15139 = CARTESIAN_POINT ( 'NONE',  ( -66.56323152365561668, 80.34130291867722917, -167.1454815528550739 ) ) ;
#15140 = FACE_OUTER_BOUND ( 'NONE', #16788, .T. ) ;
#15141 = CARTESIAN_POINT ( 'NONE',  ( -46.03642545851251100, 84.22855780814606419, -28.00000000000000355 ) ) ;
#15142 = DIRECTION ( 'NONE',  ( -0.000000000000000000, 0.000000000000000000, 1.000000000000000000 ) ) ;
#15143 = ORIENTED_EDGE ( 'NONE', *, *, #17838, .F. ) ;
#15144 = PRODUCT_RELATED_PRODUCT_CATEGORY ( 'part', '', ( #18381 ) ) ;
#15145 = DIRECTION ( 'NONE',  ( 0.9396926207859171987, 0.3420201433256445100, 4.890320548438495251E-16 ) ) ;
#15146 = CARTESIAN_POINT ( 'NONE',  ( -68.99615306438099083, 42.85071613813028790, -15.00000000000001421 ) ) ;
#15147 = ORIENTED_EDGE ( 'NONE', *, *, #3300, .F. ) ;
#15148 = EDGE_CURVE ( 'NONE', #8149, #13790, #6553, .T. ) ;
#15149 = DIRECTION ( 'NONE',  ( 0.000000000000000000, 1.000000000000000000, 0.000000000000000000 ) ) ;
#15150 = FACE_OUTER_BOUND ( 'NONE', #1795, .T. ) ;
#15151 = VERTEX_POINT ( 'NONE', #2343 ) ;
#15152 = VERTEX_POINT ( 'NONE', #5336 ) ;
#15153 = EDGE_LOOP ( 'NONE', ( #12697, #14541, #9696, #14520 ) ) ;
#15154 = DIRECTION ( 'NONE',  ( -1.000000000000000000, 0.000000000000000000, 1.692578276882434470E-16 ) ) ;
#15155 = CARTESIAN_POINT ( 'NONE',  ( -57.08002265617300708, 84.22855780814606419, 15.00000000000006928 ) ) ;
#15156 = CARTESIAN_POINT ( 'NONE',  ( -106.3193689061042164, 112.6569076202650450, 92.50000000000000000 ) ) ;
#15157 = PLANE ( 'NONE',  #3355 ) ;
#15158 = DIRECTION ( 'NONE',  ( -0.9396926207859069846, 0.3420201433256723766, 0.000000000000000000 ) ) ;
#15159 = CARTESIAN_POINT ( 'NONE',  ( 0.06682554136340505824, 4.993536075455400791, -4.350941807883202728 ) ) ;
#15160 = APPLICATION_CONTEXT ( 'automotive_design' ) ;
#15161 = ORIENTED_EDGE ( 'NONE', *, *, #14440, .F. ) ;
#15162 = CARTESIAN_POINT ( 'NONE',  ( -68.99615306438086293, 89.97460588813027016, -15.00000000000001421 ) ) ;
#15163 = CARTESIAN_POINT ( 'NONE',  ( -56.80760832784252301, 71.73152654333280509, 15.00000000000006928 ) ) ;
#15165 = ORIENTED_EDGE ( 'NONE', *, *, #2184, .T. ) ;
#15164 = DIRECTION ( 'NONE',  ( 0.000000000000000000, 0.000000000000000000, -1.000000000000000000 ) ) ;
#15166 = DIRECTION ( 'NONE',  ( 0.000000000000000000, 0.000000000000000000, -1.000000000000000000 ) ) ;
#15167 = CARTESIAN_POINT ( 'NONE',  ( -68.12361985383350316, 84.22855780814606419, -61.50000000000001421 ) ) ;
#15168 = VECTOR ( 'NONE', #11451, 1000.000000000000227 ) ;
#15169 = ORIENTED_EDGE ( 'NONE', *, *, #10075, .T. ) ;
#15170 = DIRECTION ( 'NONE',  ( -1.000000000000000000, 0.000000000000000000, 0.000000000000000000 ) ) ;
#15171 = ORIENTED_EDGE ( 'NONE', *, *, #17249, .T. ) ;
#15172 = EDGE_CURVE ( 'NONE', #11369, #4264, #3760, .T. ) ;
#15173 = ORIENTED_EDGE ( 'NONE', *, *, #17259, .F. ) ;
#15174 = SURFACE_STYLE_USAGE ( .BOTH. , #10697 ) ;
#15175 = AXIS2_PLACEMENT_3D ( 'NONE', #18328, #5500, #16913 ) ;
#15176 = DIRECTION ( 'NONE',  ( 0.3420201433256444545, -0.9396926207859171987, 0.000000000000000000 ) ) ;
#15177 = LINE ( 'NONE', #2576, #14421 ) ;
#15178 = ORIENTED_EDGE ( 'NONE', *, *, #14267, .F. ) ;
#15179 = PRODUCT_CONTEXT ( 'NONE', #9441, 'mechanical' ) ;
#15180 = CARTESIAN_POINT ( 'NONE',  ( -57.08002265617300708, 84.22855780814606419, -167.1454815528550739 ) ) ;
#15181 = EDGE_CURVE ( 'NONE', #15061, #4999, #13771, .T. ) ;
#15182 = DIRECTION ( 'NONE',  ( 0.000000000000000000, 0.000000000000000000, 1.000000000000000000 ) ) ;
#15183 = EDGE_LOOP ( 'NONE', ( #22, #3728, #15838, #915 ) ) ;
#15184 = DIRECTION ( 'NONE',  ( 1.000000000000000000, 0.000000000000000000, 5.077734830647302671E-16 ) ) ;
#15185 = DIRECTION ( 'NONE',  ( 0.3420201433256649937, -0.9396926207859097602, 0.000000000000000000 ) ) ;
#15186 = DIRECTION ( 'NONE',  ( 1.000000000000000000, 0.000000000000000000, 0.000000000000000000 ) ) ;
#15187 = VERTEX_POINT ( 'NONE', #17872 ) ;
#15188 = DIRECTION ( 'NONE',  ( 1.000000000000000000, 0.000000000000000000, 3.771137991253923150E-16 ) ) ;
#15189 = CARTESIAN_POINT ( 'NONE',  ( -102.5926225674731853, 102.8748711238780373, -20.00000000000000355 ) ) ;
#15190 = VERTEX_POINT ( 'NONE', #16650 ) ;
#15191 = LINE ( 'NONE', #3976, #172 ) ;
#15192 = VECTOR ( 'NONE', #9092, 1000.000000000000000 ) ;
#15193 = ADVANCED_FACE ( 'NONE', ( #2164 ), #9193, .F. ) ;
#15194 = EDGE_CURVE ( 'NONE', #3213, #4188, #6364, .T. ) ;
#15195 = DIRECTION ( 'NONE',  ( -0.9396926207859084279, 0.3420201433256686574, 1.086737899652989892E-16 ) ) ;
#15196 = ORIENTED_EDGE ( 'NONE', *, *, #5390, .T. ) ;
#15197 = VERTEX_POINT ( 'NONE', #16470 ) ;
#15198 = DIRECTION ( 'NONE',  ( -5.204170427930409450E-16, 0.000000000000000000, 1.000000000000000000 ) ) ;
#15199 = CARTESIAN_POINT ( 'NONE',  ( -107.5926225674731711, 57.88796029049330372, -26.35917033480641436 ) ) ;
#15200 = EDGE_CURVE ( 'NONE', #8291, #10484, #10683, .T. ) ;
#15201 = ORIENTED_EDGE ( 'NONE', *, *, #7104, .T. ) ;
#15202 = DIRECTION ( 'NONE',  ( -1.047634945911800068E-14, 0.000000000000000000, 1.000000000000000000 ) ) ;
#15203 = CARTESIAN_POINT ( 'NONE',  ( -76.88981274915232689, 77.12848153769257920, 64.92893652421413719 ) ) ;
#15204 = DIRECTION ( 'NONE',  ( 0.000000000000000000, 0.000000000000000000, 1.000000000000000000 ) ) ;
#15206 = EDGE_CURVE ( 'NONE', #3086, #6428, #2690, .T. ) ;
#15205 = VECTOR ( 'NONE', #4489, 1000.000000000000000 ) ;
#15207 = CARTESIAN_POINT ( 'NONE',  ( 97.91997734382704266, 84.22855780814606419, 55.00000000000001421 ) ) ;
#15208 = EDGE_LOOP ( 'NONE', ( #15314, #7595, #2174, #585 ) ) ;
#15209 = CARTESIAN_POINT ( 'NONE',  ( -70.71978124295696944, -96.08423613455721579, 5.204170427930421283E-15 ) ) ;
#15210 = AXIS2_PLACEMENT_3D ( 'NONE', #17352, #1832, #518 ) ;
#15211 = CYLINDRICAL_SURFACE ( 'NONE', #8839, 4.600000000000006750 ) ;
#15212 = ADVANCED_FACE ( 'NONE', ( #9464 ), #15259, .F. ) ;
#15213 = CARTESIAN_POINT ( 'NONE',  ( -68.99615306438077766, 114.4924912316626688, -167.1454815528550739 ) ) ;
#15214 = ADVANCED_FACE ( 'NONE', ( #15072 ), #7782, .T. ) ;
#15215 = DIRECTION ( 'NONE',  ( 0.000000000000000000, 0.000000000000000000, 1.000000000000000000 ) ) ;
#15216 = DIRECTION ( 'NONE',  ( -0.000000000000000000, -1.000000000000000000, -0.000000000000000000 ) ) ;
#15217 = ORIENTED_EDGE ( 'NONE', *, *, #3925, .T. ) ;
#15218 = LINE ( 'NONE', #9238, #16863 ) ;
#15219 = CARTESIAN_POINT ( 'NONE',  ( -60.58685171690505200, -91.10977296152353233, 39.65137083761684522 ) ) ;
#15220 = ORIENTED_EDGE ( 'NONE', *, *, #5730, .T. ) ;
#15221 = EDGE_CURVE ( 'NONE', #1636, #1562, #12182, .T. ) ;
#15222 = EDGE_CURVE ( 'NONE', #11183, #10943, #12382, .T. ) ;
#15223 = FACE_OUTER_BOUND ( 'NONE', #13704, .T. ) ;
#15224 = CARTESIAN_POINT ( 'NONE',  ( -36.93791207748871841, 78.13360439242255495, 66.87729283127455915 ) ) ;
#15225 = ORIENTED_EDGE ( 'NONE', *, *, #2932, .F. ) ;
#15226 = AXIS2_PLACEMENT_3D ( 'NONE', #2586, #9490, #6974 ) ;
#15227 = VERTEX_POINT ( 'NONE', #10968 ) ;
#15228 = CIRCLE ( 'NONE', #7759, 1.000000000000000888 ) ;
#15229 = DIRECTION ( 'NONE',  ( -0.9396926207859083169, 0.3420201433256687129, 0.000000000000000000 ) ) ;
#15230 = VERTEX_POINT ( 'NONE', #774 ) ;
#15231 = CARTESIAN_POINT ( 'NONE',  ( -7.840676406241780860, 112.6569076202650308, 102.5000000000000000 ) ) ;
#15232 = CARTESIAN_POINT ( 'NONE',  ( -75.01613753673549922, 60.97256703306408809, 23.80938688424596350 ) ) ;
#15233 = CARTESIAN_POINT ( 'NONE',  ( -66.19006831724836104, 58.19665835547753119, -27.99999999999999645 ) ) ;
#15234 = CARTESIAN_POINT ( 'NONE',  ( -107.5926225674731711, 57.88796029049330372, -30.35917033480640370 ) ) ;
#15235 = CYLINDRICAL_SURFACE ( 'NONE', #3738, 4.599999999999999645 ) ;
#15236 = CARTESIAN_POINT ( 'NONE',  ( -71.24615306438067819, 145.0894847045637732, -167.1454815528550739 ) ) ;
#15237 = DIRECTION ( 'NONE',  ( 1.000000000000000000, 0.000000000000000000, 0.000000000000000000 ) ) ;
#15238 = ORIENTED_EDGE ( 'NONE', *, *, #3089, .T. ) ;
#15239 = AXIS2_PLACEMENT_3D ( 'NONE', #9947, #11271, #16957 ) ;
#15240 = ADVANCED_FACE ( 'NONE', ( #9552 ), #2075, .F. ) ;
#15241 = CARTESIAN_POINT ( 'NONE',  ( -70.88454472225026848, 58.29032118345796931, -22.35917033480642502 ) ) ;
#15242 = AXIS2_PLACEMENT_3D ( 'NONE', #4116, #2525, #8233 ) ;
#15243 = VECTOR ( 'NONE', #14408, 1000.000000000000000 ) ;
#15244 = CARTESIAN_POINT ( 'NONE',  ( -71.24615306438120399, -0.3126479347707321610, -167.1454815528550739 ) ) ;
#15245 = VERTEX_POINT ( 'NONE', #2260 ) ;
#15246 = LINE ( 'NONE', #6542, #1067 ) ;
#15247 = VERTEX_POINT ( 'NONE', #17971 ) ;
#15248 = ORIENTED_EDGE ( 'NONE', *, *, #13705, .F. ) ;
#15249 = CIRCLE ( 'NONE', #11960, 4.599999999999992539 ) ;
#15250 = AXIS2_PLACEMENT_3D ( 'NONE', #11146, #18154, #10854 ) ;
#15251 = ORIENTED_EDGE ( 'NONE', *, *, #18348, .T. ) ;
#15252 = UNCERTAINTY_MEASURE_WITH_UNIT (LENGTH_MEASURE( 1.000000000000000082E-05 ), #14833, 'distance_accuracy_value', 'NONE');
#15253 = AXIS2_PLACEMENT_3D ( 'NONE', #11678, #1578, #17466 ) ;
#15254 = AXIS2_PLACEMENT_3D ( 'NONE', #5502, #10002, #14220 ) ;
#15255 = LINE ( 'NONE', #2442, #18066 ) ;
#15256 = CARTESIAN_POINT ( 'NONE',  ( -71.24615306438114715, 12.25372266522925457, 15.00000000000006928 ) ) ;
#15257 = DIRECTION ( 'NONE',  ( 1.000000000000000000, 0.000000000000000000, 0.000000000000000000 ) ) ;
#15258 = PLANE ( 'NONE',  #95 ) ;
#15259 = PLANE ( 'NONE',  #16108 ) ;
#15260 = CARTESIAN_POINT ( 'NONE',  ( -67.13262496892538422, 91.65790412808873100, 15.00000000000006928 ) ) ;
#15261 = VERTEX_POINT ( 'NONE', #2733 ) ;
#15262 = CARTESIAN_POINT ( 'NONE',  ( -71.24615306438094819, 65.66079771522920794, -15.00000000000001421 ) ) ;
#15263 = DIRECTION ( 'NONE',  ( 0.000000000000000000, 0.000000000000000000, 1.000000000000000000 ) ) ;
#15265 = ORIENTED_EDGE ( 'NONE', *, *, #3196, .F. ) ;
#15264 = LINE ( 'NONE', #4949, #14725 ) ;
#15266 = AXIS2_PLACEMENT_3D ( 'NONE', #496, #14533, #10601 ) ;
#15267 = CARTESIAN_POINT ( 'NONE',  ( -71.24615306438106188, 34.24487121522926003, -15.00000000000001421 ) ) ;
#15268 = FACE_OUTER_BOUND ( 'NONE', #948, .T. ) ;
#15269 = VERTEX_POINT ( 'NONE', #1240 ) ;
#15270 = AXIS2_PLACEMENT_3D ( 'NONE', #16882, #12694, #11285 ) ;
#15271 = AXIS2_PLACEMENT_3D ( 'NONE', #10902, #701, #2276 ) ;
#15272 = LINE ( 'NONE', #13784, #3824 ) ;
#15273 = ORIENTED_EDGE ( 'NONE', *, *, #15890, .F. ) ;
#15274 = EDGE_CURVE ( 'NONE', #11154, #1345, #5436, .T. ) ;
#15275 = ORIENTED_EDGE ( 'NONE', *, *, #4239, .F. ) ;
#15276 = AXIS2_PLACEMENT_3D ( 'NONE', #5811, #4059, #10119 ) ;
#15277 =( NAMED_UNIT ( * ) PLANE_ANGLE_UNIT ( ) SI_UNIT ( $, .RADIAN. ) );
#15278 = FACE_OUTER_BOUND ( 'NONE', #3478, .T. ) ;
#15279 = CARTESIAN_POINT ( 'NONE',  ( -71.24615306438086293, 94.82400230456377699, -167.1454815528550739 ) ) ;
#15280 = ORIENTED_EDGE ( 'NONE', *, *, #3878, .T. ) ;
#15281 = VECTOR ( 'NONE', #13401, 1000.000000000000000 ) ;
#15282 = CARTESIAN_POINT ( 'NONE',  ( -31.57667891805219895, -91.08423613455724421, 10.52509945732312957 ) ) ;
#15283 = LINE ( 'NONE', #16673, #8197 ) ;
#15284 = VERTEX_POINT ( 'NONE', #2835 ) ;
#15285 = FACE_OUTER_BOUND ( 'NONE', #13631, .T. ) ;
#15286 = LINE ( 'NONE', #9579, #2727 ) ;
#15287 = DIRECTION ( 'NONE',  ( 0.000000000000000000, 0.000000000000000000, 1.000000000000000000 ) ) ;
#15288 = ORIENTED_EDGE ( 'NONE', *, *, #6866, .F. ) ;
#15289 = FACE_BOUND ( 'NONE', #1071, .T. ) ;
#15290 = CARTESIAN_POINT ( 'NONE',  ( -76.37409655828275845, -91.08423613455721579, 28.18308811886536347 ) ) ;
#15291 = VERTEX_POINT ( 'NONE', #15740 ) ;
#15292 = AXIS2_PLACEMENT_3D ( 'NONE', #4286, #15958, #9996 ) ;
#15293 = FACE_OUTER_BOUND ( 'NONE', #1347, .T. ) ;
#15294 = LINE ( 'NONE', #8483, #4608 ) ;
#15295 = CIRCLE ( 'NONE', #17980, 6.500000000000039968 ) ;
#15296 = EDGE_LOOP ( 'NONE', ( #15178, #16018, #10985, #16361 ) ) ;
#15297 = ADVANCED_FACE ( 'NONE', ( #4227 ), #1513, .T. ) ;
#15298 = ORIENTED_EDGE ( 'NONE', *, *, #14790, .T. ) ;
#15299 = DIRECTION ( 'NONE',  ( 0.000000000000000000, 0.000000000000000000, 1.000000000000000000 ) ) ;
#15300 = EDGE_LOOP ( 'NONE', ( #15487, #7615, #16472, #9389 ) ) ;
#15301 = CARTESIAN_POINT ( 'NONE',  ( 5.233202738124664855, -111.0842361345572158, -57.00000000000000000 ) ) ;
#15302 = CARTESIAN_POINT ( 'NONE',  ( -68.99615306438089135, 83.07656473166271383, -15.00000000000001421 ) ) ;
#15303 = CARTESIAN_POINT ( 'NONE',  ( -45.21333244822126574, 88.15687341518456321, -167.1454815528550739 ) ) ;
#15304 = DIRECTION ( 'NONE',  ( 0.000000000000000000, 0.000000000000000000, -1.000000000000000000 ) ) ;
#15305 = EDGE_LOOP ( 'NONE', ( #7971, #10212, #7368, #664 ) ) ;
#15306 = EDGE_CURVE ( 'NONE', #17985, #14706, #16853, .T. ) ;
#15307 = DIRECTION ( 'NONE',  ( 1.000000000000000000, 0.000000000000000000, 0.000000000000000000 ) ) ;
#15308 = VECTOR ( 'NONE', #18199, 1000.000000000000000 ) ;
#15309 = VECTOR ( 'NONE', #406, 1000.000000000000000 ) ;
#15310 = CARTESIAN_POINT ( 'NONE',  ( -46.36441787118067026, 82.83016482797245317, -15.00000000000001421 ) ) ;
#15311 = DIRECTION ( 'NONE',  ( -1.000000000000000000, 0.000000000000000000, 1.692578276882434470E-16 ) ) ;
#15312 = CARTESIAN_POINT ( 'NONE',  ( -71.24615306438080609, 116.8151508545637114, -167.1454815528550739 ) ) ;
#15313 = DIRECTION ( 'NONE',  ( -0.9396926207859171987, 0.3420201433256445100, -4.890320548438495251E-16 ) ) ;
#15314 = ORIENTED_EDGE ( 'NONE', *, *, #16346, .F. ) ;
#15315 = DIRECTION ( 'NONE',  ( -0.9396926207859069846, 0.3420201433256723766, 0.000000000000000000 ) ) ;
#15316 = CARTESIAN_POINT ( 'NONE',  ( -62.92154743286889129, -91.96845925178436687, 42.55229934223208943 ) ) ;
#15317 = CIRCLE ( 'NONE', #11155, 4.599999999999999645 ) ;
#15318 = CARTESIAN_POINT ( 'NONE',  ( -71.24615306438114715, 9.112130015229229940, 15.00000000000006928 ) ) ;
#15319 = EDGE_CURVE ( 'NONE', #626, #11065, #14044, .T. ) ;
#15320 = CARTESIAN_POINT ( 'NONE',  ( -36.17229811368392944, 81.79799583099489269, 69.61205705513911823 ) ) ;
#15321 = VERTEX_POINT ( 'NONE', #14250 ) ;
#15322 = EDGE_CURVE ( 'NONE', #7705, #14872, #8442, .T. ) ;
#15323 = ORIENTED_EDGE ( 'NONE', *, *, #989, .F. ) ;
#15324 = EDGE_CURVE ( 'NONE', #3332, #6312, #8257, .T. ) ;
#15325 = VECTOR ( 'NONE', #9445, 1000.000000000000227 ) ;
#15326 = VECTOR ( 'NONE', #3800, 1000.000000000000000 ) ;
#15327 = AXIS2_PLACEMENT_3D ( 'NONE', #925, #10944, #17848 ) ;
#15328 = DIRECTION ( 'NONE',  ( 0.9396926207859078728, 0.3420201433256701007, 0.000000000000000000 ) ) ;
#15329 = ORIENTED_EDGE ( 'NONE', *, *, #10663, .F. ) ;
#15330 = CARTESIAN_POINT ( 'NONE',  ( -97.59262256747321373, 117.8748711238780515, -25.00000000000000000 ) ) ;
#15331 = PLANE ( 'NONE',  #15017 ) ;
#15332 = DIRECTION ( 'NONE',  ( 1.000000000000000000, 0.000000000000000000, 0.000000000000000000 ) ) ;
#15333 = VERTEX_POINT ( 'NONE', #12669 ) ;
#15334 = EDGE_CURVE ( 'NONE', #8291, #3371, #14332, .T. ) ;
#15335 = AXIS2_PLACEMENT_3D ( 'NONE', #13486, #17782, #7685 ) ;
#15336 = CIRCLE ( 'NONE', #9066, 12.50000000000000355 ) ;
#15337 = EDGE_CURVE ( 'NONE', #9366, #8099, #1343, .T. ) ;
#15338 = CARTESIAN_POINT ( 'NONE',  ( -31.03642545851250745, 84.22855780814606419, 28.00000000000000355 ) ) ;
#15339 = EDGE_CURVE ( 'NONE', #10505, #7990, #15541, .T. ) ;
#15340 = LINE ( 'NONE', #838, #6409 ) ;
#15341 = CARTESIAN_POINT ( 'NONE',  ( -57.08002265617300708, 84.22855780814606419, 37.50000000000000000 ) ) ;
#15342 = DIRECTION ( 'NONE',  ( 1.558623840612994987E-16, 1.000000000000000000, 0.000000000000000000 ) ) ;
#15343 = ORIENTED_EDGE ( 'NONE', *, *, #11815, .F. ) ;
#15344 = PLANE ( 'NONE',  #15650 ) ;
#15345 = VECTOR ( 'NONE', #17338, 1000.000000000000227 ) ;
#15346 = AXIS2_PLACEMENT_3D ( 'NONE', #1382, #5294, #16792 ) ;
#15347 = DIRECTION ( 'NONE',  ( 8.326672684688674053E-15, 0.000000000000000000, -1.000000000000000000 ) ) ;
#15348 = ORIENTED_EDGE ( 'NONE', *, *, #10420, .T. ) ;
#15349 = EDGE_CURVE ( 'NONE', #14316, #14366, #9654, .T. ) ;
#15350 = CARTESIAN_POINT ( 'NONE',  ( -98.90286936182239685, -111.0842361345572158, 5.654315315325477265 ) ) ;
#15351 = CARTESIAN_POINT ( 'NONE',  ( -92.59262256747318531, 0.3328663868096687350, 25.00000000000000000 ) ) ;
#15352 = EDGE_LOOP ( 'NONE', ( #12833, #7377, #10055 ) ) ;
#15353 = EDGE_LOOP ( 'NONE', ( #6584, #15024, #1196, #14895 ) ) ;
#15354 = VECTOR ( 'NONE', #852, 1000.000000000000000 ) ;
#15355 = EDGE_CURVE ( 'NONE', #9827, #11230, #13965, .T. ) ;
#15356 = EDGE_CURVE ( 'NONE', #16762, #7430, #18262, .T. ) ;
#15357 = EDGE_LOOP ( 'NONE', ( #11069, #3108, #2545, #10897, #10633, #2989, #11738, #5982, #14349, #13416, #17562, #7729, #11783, #13731, #11762, #4728 ) ) ;
#15358 = AXIS2_PLACEMENT_3D ( 'NONE', #6801, #11016, #7825 ) ;
#15359 = VECTOR ( 'NONE', #13962, 1000.000000000000000 ) ;
#15360 = FACE_OUTER_BOUND ( 'NONE', #744, .T. ) ;
#15361 = CARTESIAN_POINT ( 'NONE',  ( -70.71978124295696944, -91.08423613455721579, 5.204170427930421283E-15 ) ) ;
#15362 = DIRECTION ( 'NONE',  ( -1.000000000000000000, 0.000000000000000000, 0.000000000000000000 ) ) ;
#15363 = DIRECTION ( 'NONE',  ( -0.9396926207859158664, 0.3420201433256481738, 1.086737899652998397E-16 ) ) ;
#15364 = CARTESIAN_POINT ( 'NONE',  ( -68.99615306438117557, 1.395155831662692192, 15.00000000000006928 ) ) ;
#15365 = PLANE ( 'NONE',  #5125 ) ;
#15366 = VERTEX_POINT ( 'NONE', #4054 ) ;
#15367 = CLOSED_SHELL ( 'NONE', ( #7673, #15552, #951, #3210, #5740, #570, #4630, #6493, #7543, #10204, #12372, #8260, #1628, #13664, #712, #3440, #10639, #17455, #17285, #14877, #2779, #2273, #18121, #16580, #8473, #81, #487, #14194, #16680, #9961, #802, #13954, #10636, #11641, #1841, #13727, #15710, #10006, #9519, #6709, #7102, #2085, #11583, #4460, #4464, #15193, #5607, #1710, #2065, #10387, #2063, #14624, #561, #1700, #2292, #18407, #17604, #14650, #144, #2308, #6246, #4677, #15908, #15461, #15554, #12109, #7841, #5940, #9391, #9911, #14326, #3772, #7213, #14945, #3102, #9499, #11990, #5147, #15113, #16811, #9385, #2769, #27, #9728, #8929 ) ) ;
#15368 = FACE_OUTER_BOUND ( 'NONE', #10977, .T. ) ;
#15369 = CYLINDRICAL_SURFACE ( 'NONE', #7510, 9.999999999999994671 ) ;
#15371 = ORIENTED_EDGE ( 'NONE', *, *, #3198, .F. ) ;
#15370 = CARTESIAN_POINT ( 'NONE',  ( -78.05523331206480009, 85.94077383471115184, 69.80605996636154487 ) ) ;
#15372 = DIRECTION ( 'NONE',  ( 0.000000000000000000, 1.000000000000000000, -1.779758311459928026E-16 ) ) ;
#15373 = CARTESIAN_POINT ( 'NONE',  ( -127.5926225674731711, 57.88796029049329661, 22.35917033480642502 ) ) ;
#15374 = EDGE_LOOP ( 'NONE', ( #2616, #7424, #13913, #2849 ) ) ;
#15375 = VECTOR ( 'NONE', #8193, 1000.000000000000000 ) ;
#15376 = AXIS2_PLACEMENT_3D ( 'NONE', #15501, #11217, #7002 ) ;
#15377 = VECTOR ( 'NONE', #15182, 1000.000000000000000 ) ;
#15378 = CARTESIAN_POINT ( 'NONE',  ( -35.92682688279126779, 73.26749283227019305, 102.5000000000000000 ) ) ;
#15380 = ORIENTED_EDGE ( 'NONE', *, *, #1506, .T. ) ;
#15379 = VECTOR ( 'NONE', #5969, 1000.000000000000000 ) ;
#15381 = PRODUCT_DEFINITION_SHAPE ( 'NONE', 'NONE',  #18528 ) ;
#15382 = ORIENTED_EDGE ( 'NONE', *, *, #1707, .T. ) ;
#15383 = VECTOR ( 'NONE', #15564, 1000.000000000000000 ) ;
#15384 = DIRECTION ( 'NONE',  ( -0.000000000000000000, -0.000000000000000000, -1.000000000000000000 ) ) ;
#15385 = CARTESIAN_POINT ( 'NONE',  ( -49.75809927370887920, 76.28065702765852052, 15.00000000000006928 ) ) ;
#15386 = VECTOR ( 'NONE', #16404, 1000.000000000000114 ) ;
#15387 = ORIENTED_EDGE ( 'NONE', *, *, #3189, .F. ) ;
#15388 = SHAPE_DEFINITION_REPRESENTATION ( #11040, #16862 ) ;
#15389 = ORIENTED_EDGE ( 'NONE', *, *, #9149, .F. ) ;
#15390 = CARTESIAN_POINT ( 'NONE',  ( -28.96456321416951596, 53.44918566155911321, -24.93391072407674613 ) ) ;
#15391 = CARTESIAN_POINT ( 'NONE',  ( -65.06546592763146464, -91.08423613455721579, 45.05044770573184110 ) ) ;
#15392 = ORIENTED_EDGE ( 'NONE', *, *, #11920, .F. ) ;
#15393 = DIRECTION ( 'NONE',  ( 0.000000000000000000, 1.000000000000000000, 0.000000000000000000 ) ) ;
#15394 = CARTESIAN_POINT ( 'NONE',  ( -71.24615306438094819, 65.66079771522920794, -167.1454815528550739 ) ) ;
#15395 = PLANE ( 'NONE',  #6645 ) ;
#15396 = ORIENTED_EDGE ( 'NONE', *, *, #6169, .T. ) ;
#15397 = FACE_OUTER_BOUND ( 'NONE', #10356, .T. ) ;
#15398 = DIRECTION ( 'NONE',  ( -5.204170427930409450E-16, 0.000000000000000000, 1.000000000000000000 ) ) ;
#15400 = ORIENTED_EDGE ( 'NONE', *, *, #16993, .F. ) ;
#15399 = PRODUCT_DEFINITION ( 'UNKNOWN', '', #8493, #8336 ) ;
#15401 = LINE ( 'NONE', #15587, #16872 ) ;
#15402 = VECTOR ( 'NONE', #846, 1000.000000000000000 ) ;
#15403 = EDGE_CURVE ( 'NONE', #15435, #5779, #15228, .T. ) ;
#15404 = CARTESIAN_POINT ( 'NONE',  ( -68.99615306438111872, 20.24471173166267235, -15.00000000000001421 ) ) ;
#15405 = VECTOR ( 'NONE', #8302, 1000.000000000000000 ) ;
#15406 = ORIENTED_EDGE ( 'NONE', *, *, #9786, .T. ) ;
#15407 = VECTOR ( 'NONE', #2501, 1000.000000000000000 ) ;
#15408 = ORIENTED_EDGE ( 'NONE', *, *, #2186, .T. ) ;
#15409 = CARTESIAN_POINT ( 'NONE',  ( -70.27900850916093134, -47.21335801510345220, -15.00000000000001599 ) ) ;
#15410 = CARTESIAN_POINT ( 'NONE',  ( 45.30000000000000426, 0.000000000000000000, 0.000000000000000000 ) ) ;
#15411 = ORIENTED_EDGE ( 'NONE', *, *, #1943, .F. ) ;
#15412 = CARTESIAN_POINT ( 'NONE',  ( -53.84898691462515785, 93.95493478196527803, 15.00000000000006928 ) ) ;
#15413 = DIRECTION ( 'NONE',  ( 0.000000000000000000, 0.000000000000000000, 1.000000000000000000 ) ) ;
#15414 = CARTESIAN_POINT ( 'NONE',  ( -66.35137518009933899, 89.78028827820979529, -15.00000000000001421 ) ) ;
#15415 = PLANE ( 'NONE',  #18048 ) ;
#15416 = ORIENTED_EDGE ( 'NONE', *, *, #17516, .T. ) ;
#15417 = LINE ( 'NONE', #2603, #17052 ) ;
#15418 = AXIS2_PLACEMENT_3D ( 'NONE', #4748, #3354, #6791 ) ;
#15419 = FACE_OUTER_BOUND ( 'NONE', #11758, .T. ) ;
#15420 = AXIS2_PLACEMENT_3D ( 'NONE', #15727, #265, #4557 ) ;
#15421 = CARTESIAN_POINT ( 'NONE',  ( -68.99615306438117557, 2.010011688130281193, -167.1454815528550739 ) ) ;
#15422 = CARTESIAN_POINT ( 'NONE',  ( 9.727308505134775629, 10.18372637758682764, 47.32161794854564363 ) ) ;
#15423 = VERTEX_POINT ( 'NONE', #9760 ) ;
#15424 = DIRECTION ( 'NONE',  ( 0.3420201433256481738, 0.9396926207859158664, -0.000000000000000000 ) ) ;
#15425 = DIRECTION ( 'NONE',  ( 0.000000000000000000, 0.000000000000000000, -1.000000000000000000 ) ) ;
#15426 = DIRECTION ( 'NONE',  ( 0.000000000000000000, 1.000000000000000000, 0.000000000000000000 ) ) ;
#15427 = SURFACE_STYLE_USAGE ( .BOTH. , #8220 ) ;
#15428 = ORIENTED_EDGE ( 'NONE', *, *, #3079, .T. ) ;
#15429 = ORIENTED_EDGE ( 'NONE', *, *, #809, .F. ) ;
#15430 = EDGE_CURVE ( 'NONE', #11979, #8996, #12845, .T. ) ;
#15431 = PLANE ( 'NONE',  #5175 ) ;
#15432 = LINE ( 'NONE', #6819, #14196 ) ;
#15433 = FACE_OUTER_BOUND ( 'NONE', #13736, .T. ) ;
#15434 = LINE ( 'NONE', #15139, #12977 ) ;
#15435 = VERTEX_POINT ( 'NONE', #12941 ) ;
#15436 = CARTESIAN_POINT ( 'NONE',  ( 0.4053525175236978306, 3.145852061456188675, -6.500000000000061284 ) ) ;
#15437 = DIRECTION ( 'NONE',  ( -0.000000000000000000, -0.000000000000000000, -1.000000000000000000 ) ) ;
#15438 = DIRECTION ( 'NONE',  ( 0.000000000000000000, 0.000000000000000000, 1.000000000000000000 ) ) ;
#15439 = CARTESIAN_POINT ( 'NONE',  ( -100.4870060002411805, -151.5628872026273086, -57.00000000000000000 ) ) ;
#15440 = VERTEX_POINT ( 'NONE', #109 ) ;
#15441 = EDGE_CURVE ( 'NONE', #15932, #11023, #5807, .T. ) ;
#15442 = EDGE_CURVE ( 'NONE', #16069, #5776, #18367, .T. ) ;
#15443 = FACE_OUTER_BOUND ( 'NONE', #7808, .T. ) ;
#15444 = ORIENTED_EDGE ( 'NONE', *, *, #18104, .T. ) ;
#15445 = CARTESIAN_POINT ( 'NONE',  ( -71.24615306438079188, 110.5319655545637403, -15.00000000000001421 ) ) ;
#15446 = CARTESIAN_POINT ( 'NONE',  ( -71.24615306438114715, 13.14259340456377956, -167.1454815528550739 ) ) ;
#15447 = ORIENTED_EDGE ( 'NONE', *, *, #8714, .F. ) ;
#15448 = ORIENTED_EDGE ( 'NONE', *, *, #1499, .F. ) ;
#15449 = EDGE_CURVE ( 'NONE', #6428, #3086, #4756, .T. ) ;
#15450 = ADVANCED_FACE ( 'NONE', ( #9939 ), #13296, .T. ) ;
#15451 = EDGE_LOOP ( 'NONE', ( #5838, #7952, #17223, #3499 ) ) ;
#15452 = UNCERTAINTY_MEASURE_WITH_UNIT (LENGTH_MEASURE( 1.000000000000000082E-05 ), #4462, 'distance_accuracy_value', 'NONE');
#15453 = CARTESIAN_POINT ( 'NONE',  ( -71.24615306438109030, 31.10327856522923540, -15.00000000000001421 ) ) ;
#15454 = LINE ( 'NONE', #14050, #8458 ) ;
#15455 = CYLINDRICAL_SURFACE ( 'NONE', #9388, 3.999999999999989786 ) ;
#15456 = LINE ( 'NONE', #2445, #14439 ) ;
#15457 = EDGE_CURVE ( 'NONE', #8454, #12168, #10169, .T. ) ;
#15458 = CARTESIAN_POINT ( 'NONE',  ( 4.699999999999995737, -3.752776749732712691, -6.500000000000033751 ) ) ;
#15459 = DIRECTION ( 'NONE',  ( 0.000000000000000000, 0.000000000000000000, 1.000000000000000000 ) ) ;
#15460 = VERTEX_POINT ( 'NONE', #14679 ) ;
#15461 = ADVANCED_FACE ( 'NONE', ( #17302 ), #4670, .T. ) ;
#15462 = CARTESIAN_POINT ( 'NONE',  ( -68.99615306438082030, 99.39938383813029077, -15.00000000000001421 ) ) ;
#15463 = ORIENTED_EDGE ( 'NONE', *, *, #16899, .T. ) ;
#15464 = CARTESIAN_POINT ( 'NONE',  ( -97.59262256747319952, 50.58224449241411236, -25.00000000000000000 ) ) ;
#15465 = ADVANCED_FACE ( 'NONE', ( #11610 ), #3356, .T. ) ;
#15466 = EDGE_CURVE ( 'NONE', #748, #7603, #13110, .T. ) ;
#15467 = CARTESIAN_POINT ( 'NONE',  ( -70.71978124295696944, -111.0842361345572158, 5.204170427930421283E-15 ) ) ;
#15468 = VERTEX_POINT ( 'NONE', #7669 ) ;
#15469 = DIRECTION ( 'NONE',  ( 0.000000000000000000, 0.000000000000000000, 1.000000000000000000 ) ) ;
#15470 = ORIENTED_EDGE ( 'NONE', *, *, #14696, .T. ) ;
#15471 = EDGE_CURVE ( 'NONE', #11293, #16643, #8986, .T. ) ;
#15472 = VERTEX_POINT ( 'NONE', #8813 ) ;
#15473 =( NAMED_UNIT ( * ) SI_UNIT ( $, .STERADIAN. ) SOLID_ANGLE_UNIT ( ) );
#15474 = DIRECTION ( 'NONE',  ( 0.000000000000000000, 0.000000000000000000, 1.000000000000000000 ) ) ;
#15475 = DIRECTION ( 'NONE',  ( 1.000000000000000000, 0.000000000000000000, 0.000000000000000000 ) ) ;
#15476 = ORIENTED_EDGE ( 'NONE', *, *, #12631, .T. ) ;
#15477 = ORIENTED_EDGE ( 'NONE', *, *, #10526, .F. ) ;
#15478 = CARTESIAN_POINT ( 'NONE',  ( -68.99615306438077766, 114.4924912316626688, -15.00000000000001421 ) ) ;
#15479 = DIRECTION ( 'NONE',  ( 2.062304371594500494E-16, -1.000000000000000000, 0.000000000000000000 ) ) ;
#15480 = ORIENTED_EDGE ( 'NONE', *, *, #3534, .F. ) ;
#15481 = SURFACE_SIDE_STYLE ('',( #7985 ) ) ;
#15482 = DIRECTION ( 'NONE',  ( 0.000000000000000000, 0.000000000000000000, -1.000000000000000000 ) ) ;
#15483 = FACE_OUTER_BOUND ( 'NONE', #12860, .T. ) ;
#15484 = ORIENTED_EDGE ( 'NONE', *, *, #2752, .F. ) ;
#15485 = CARTESIAN_POINT ( 'NONE',  ( -73.90245058923942167, 108.3059858121137182, -23.04901498212743505 ) ) ;
#15486 = DIRECTION ( 'NONE',  ( -1.000000000000000000, -3.016910393003138520E-15, 0.000000000000000000 ) ) ;
#15487 = ORIENTED_EDGE ( 'NONE', *, *, #11005, .F. ) ;
#15488 = FACE_BOUND ( 'NONE', #4796, .T. ) ;
#15489 = CARTESIAN_POINT ( 'NONE',  ( -66.51364668169601657, 56.41604328733773599, -28.00000000000000355 ) ) ;
#15490 = ORIENTED_EDGE ( 'NONE', *, *, #7806, .F. ) ;
#15491 = AXIS2_PLACEMENT_3D ( 'NONE', #15829, #8826, #4594 ) ;
#15492 = ORIENTED_EDGE ( 'NONE', *, *, #13073, .F. ) ;
#15493 = DIRECTION ( 'NONE',  ( 0.000000000000000000, 1.000000000000000000, 0.000000000000000000 ) ) ;
#15494 = ORIENTED_EDGE ( 'NONE', *, *, #9164, .F. ) ;
#15495 = CARTESIAN_POINT ( 'NONE',  ( -71.24615306438094819, 65.66079771522920794, 15.00000000000006928 ) ) ;
#15496 = DIRECTION ( 'NONE',  ( 0.000000000000000000, 0.000000000000000000, -1.000000000000000000 ) ) ;
#15497 = DIRECTION ( 'NONE',  ( -1.000000000000000000, 0.000000000000000000, 1.387778780781445182E-16 ) ) ;
#15498 = LINE ( 'NONE', #9797, #8512 ) ;
#15499 = ORIENTED_EDGE ( 'NONE', *, *, #17838, .T. ) ;
#15500 = DIRECTION ( 'NONE',  ( -0.000000000000000000, 0.000000000000000000, -1.000000000000000000 ) ) ;
#15501 = CARTESIAN_POINT ( 'NONE',  ( -71.24615306438100504, 50.84170520456370923, -167.1454815528550739 ) ) ;
#15502 = DIRECTION ( 'NONE',  ( 1.000000000000000000, 0.000000000000000000, 0.000000000000000000 ) ) ;
#15503 = AXIS2_PLACEMENT_3D ( 'NONE', #7767, #9000, #14786 ) ;
#15504 = CARTESIAN_POINT ( 'NONE',  ( -68.99615306438072082, 130.2004544816626890, -15.00000000000001421 ) ) ;
#15505 = PLANE ( 'NONE',  #6010 ) ;
#15506 = VERTEX_POINT ( 'NONE', #10469 ) ;
#15507 = CARTESIAN_POINT ( 'NONE',  ( -68.99615306438094819, 64.22700883166265839, -15.00000000000001421 ) ) ;
#15508 = PLANE ( 'NONE',  #18490 ) ;
#15509 = DIRECTION ( 'NONE',  ( -0.000000000000000000, -0.000000000000000000, -1.000000000000000000 ) ) ;
#15510 = DIRECTION ( 'NONE',  ( 0.000000000000000000, 0.000000000000000000, 1.000000000000000000 ) ) ;
#15511 = ORIENTED_EDGE ( 'NONE', *, *, #17156, .F. ) ;
#15512 = ORIENTED_EDGE ( 'NONE', *, *, #17197, .F. ) ;
#15513 = VECTOR ( 'NONE', #18124, 1000.000000000000000 ) ;
#15515 = EDGE_CURVE ( 'NONE', #2577, #1230, #10116, .T. ) ;
#15514 = DIRECTION ( 'NONE',  ( 1.000000000000000000, 0.000000000000000000, -0.000000000000000000 ) ) ;
#15516 = EDGE_LOOP ( 'NONE', ( #3778, #1760, #17983, #6574 ) ) ;
#15517 = CARTESIAN_POINT ( 'NONE',  ( -64.89435165812551531, 90.86016871721213306, -167.1454815528550739 ) ) ;
#15518 = CARTESIAN_POINT ( 'NONE',  ( -44.59353464447068660, 84.80960611389554060, -167.1454815528550739 ) ) ;
#15519 = CARTESIAN_POINT ( 'NONE',  ( -71.24615306438109030, 27.96168591522921076, 15.00000000000006928 ) ) ;
#15520 = VERTEX_POINT ( 'NONE', #3096 ) ;
#15521 = CARTESIAN_POINT ( 'NONE',  ( -67.15738250865011594, 107.7249262104797225, -28.00000000000000355 ) ) ;
#15522 = CARTESIAN_POINT ( 'NONE',  ( 0.5805565836007609004, 7.505553499465141165, -1.387778780781445676E-14 ) ) ;
#15523 = CARTESIAN_POINT ( 'NONE',  ( 5.299999999999998934, -7.505553499465293932, 1.040834085586084257E-14 ) ) ;
#15524 = CARTESIAN_POINT ( 'NONE',  ( -71.24615306438079188, 112.7846874652292399, 15.00000000000006928 ) ) ;
#15525 = PRODUCT_DEFINITION_SHAPE ( 'NONE', 'NONE',  #11622 ) ;
#15526 = ORIENTED_EDGE ( 'NONE', *, *, #15442, .F. ) ;
#15527 = ADVANCED_FACE ( 'NONE', ( #16000 ), #474, .T. ) ;
#15528 = DIRECTION ( 'NONE',  ( 0.000000000000000000, 0.000000000000000000, 1.000000000000000000 ) ) ;
#15529 = VECTOR ( 'NONE', #16100, 1000.000000000000000 ) ;
#15530 = ORIENTED_EDGE ( 'NONE', *, *, #952, .T. ) ;
#15531 = CYLINDRICAL_SURFACE ( 'NONE', #6570, 172.7605492041889192 ) ;
#15532 = VECTOR ( 'NONE', #3942, 999.9999999999998863 ) ;
#15533 = DIRECTION ( 'NONE',  ( 0.000000000000000000, 0.000000000000000000, 1.000000000000000000 ) ) ;
#15534 = EDGE_LOOP ( 'NONE', ( #16545, #15933, #11617, #8043 ) ) ;
#15535 = ORIENTED_EDGE ( 'NONE', *, *, #10802, .F. ) ;
#15536 = ORIENTED_EDGE ( 'NONE', *, *, #10100, .T. ) ;
#15537 = CARTESIAN_POINT ( 'NONE',  ( -70.06856178257687873, 57.88796029049330372, -22.35917033480642502 ) ) ;
#15538 = CARTESIAN_POINT ( 'NONE',  ( -107.5926225674731853, 110.5691553257988460, 26.35917033480641436 ) ) ;
#15539 = VECTOR ( 'NONE', #5137, 1000.000000000000000 ) ;
#15540 = LINE ( 'NONE', #1600, #3256 ) ;
#15541 = LINE ( 'NONE', #15364, #2376 ) ;
#15542 = VECTOR ( 'NONE', #1033, 1000.000000000000000 ) ;
#15543 = DIRECTION ( 'NONE',  ( 1.000000000000000000, 0.000000000000000000, 0.000000000000000000 ) ) ;
#15544 = ORIENTED_EDGE ( 'NONE', *, *, #13858, .F. ) ;
#15545 = EDGE_CURVE ( 'NONE', #14830, #11545, #14775, .T. ) ;
#15546 = DIRECTION ( 'NONE',  ( -1.000000000000000000, 2.888894916580850627E-30, -8.326672684688672475E-15 ) ) ;
#15547 = EDGE_LOOP ( 'NONE', ( #10111, #18227, #10860, #16724 ) ) ;
#15548 = EDGE_CURVE ( 'NONE', #10355, #18436, #15819, .T. ) ;
#15549 = DIRECTION ( 'NONE',  ( 1.156482317317869999E-16, 0.000000000000000000, 1.000000000000000000 ) ) ;
#15550 = CYLINDRICAL_SURFACE ( 'NONE', #15831, 95.91469608272775815 ) ;
#15552 = ADVANCED_FACE ( 'NONE', ( #204 ), #11704, .F. ) ;
#15551 = ORIENTED_EDGE ( 'NONE', *, *, #2516, .F. ) ;
#15553 = SHAPE_REPRESENTATION ( 'Gear Rack', ( #16217 ), #11478 ) ;
#15554 = ADVANCED_FACE ( 'NONE', ( #4749 ), #14422, .T. ) ;
#15555 = VECTOR ( 'NONE', #8309, 1000.000000000000114 ) ;
#15556 = CARTESIAN_POINT ( 'NONE',  ( -91.19225650277898865, 92.96220022626712876, 102.5000000000000000 ) ) ;
#15557 = ORIENTED_EDGE ( 'NONE', *, *, #8572, .T. ) ;
#15558 = VECTOR ( 'NONE', #6450, 1000.000000000000000 ) ;
#15560 = EDGE_CURVE ( 'NONE', #7091, #7155, #9878, .T. ) ;
#15559 = AXIS2_PLACEMENT_3D ( 'NONE', #16056, #7290, #1489 ) ;
#15561 = EDGE_CURVE ( 'NONE', #455, #2538, #5890, .T. ) ;
#15562 = ORIENTED_EDGE ( 'NONE', *, *, #17734, .F. ) ;
#15563 = ADVANCED_FACE ( 'NONE', ( #7482 ), #13200, .T. ) ;
#15564 = DIRECTION ( 'NONE',  ( 0.000000000000000000, 0.000000000000000000, 1.000000000000000000 ) ) ;
#15565 = ADVANCED_FACE ( 'NONE', ( #16074 ), #753, .T. ) ;
#15566 = DIRECTION ( 'NONE',  ( 0.000000000000000000, 0.000000000000000000, -1.000000000000000000 ) ) ;
#15567 = CARTESIAN_POINT ( 'NONE',  ( -68.99615306438089135, 79.93497208166267853, -167.1454815528550739 ) ) ;
#15568 = ORIENTED_EDGE ( 'NONE', *, *, #5207, .F. ) ;
#15569 = ITEM_DEFINED_TRANSFORMATION ( 'NONE', 'NONE', #16837,  #16217 ) ;
#15570 = AXIS2_PLACEMENT_3D ( 'NONE', #18291, #2475, #8077 ) ;
#15571 = ORIENTED_EDGE ( 'NONE', *, *, #2255, .F. ) ;
#15572 = CARTESIAN_POINT ( 'NONE',  ( -71.24615306438091977, 71.94398301522919326, -167.1454815528550739 ) ) ;
#15573 = DIRECTION ( 'NONE',  ( 0.000000000000000000, 0.000000000000000000, 1.000000000000000000 ) ) ;
#15574 = ORIENTED_EDGE ( 'NONE', *, *, #13622, .F. ) ;
#15575 = EDGE_CURVE ( 'NONE', #16660, #6428, #4851, .T. ) ;
#15576 = CARTESIAN_POINT ( 'NONE',  ( -57.08002265617300708, 84.22855780814606419, -15.00000000000001421 ) ) ;
#15577 = DIRECTION ( 'NONE',  ( 1.000000000000000000, 0.000000000000000000, 0.000000000000000000 ) ) ;
#15578 = EDGE_CURVE ( 'NONE', #11425, #18012, #8064, .T. ) ;
#15579 = CARTESIAN_POINT ( 'NONE',  ( -68.99615306438086293, 89.35975003166268493, -167.1454815528550739 ) ) ;
#15580 = VECTOR ( 'NONE', #10518, 1000.000000000000000 ) ;
#15581 = EDGE_CURVE ( 'NONE', #14482, #4354, #2423, .T. ) ;
#15582 = ORIENTED_EDGE ( 'NONE', *, *, #3545, .F. ) ;
#15583 = DIRECTION ( 'NONE',  ( 0.000000000000000000, 0.000000000000000000, 1.000000000000000000 ) ) ;
#15584 = DIRECTION ( 'NONE',  ( 1.000000000000000000, 0.000000000000000000, 5.551115123125780730E-16 ) ) ;
#15585 = ORIENTED_EDGE ( 'NONE', *, *, #6042, .T. ) ;
#15586 = ADVANCED_FACE ( 'NONE', ( #8131 ), #14859, .T. ) ;
#15587 = CARTESIAN_POINT ( 'NONE',  ( -92.59262256747321373, 117.8748711238780373, 35.00000000000000000 ) ) ;
#15588 = ORIENTED_EDGE ( 'NONE', *, *, #11802, .F. ) ;
#15589 = CARTESIAN_POINT ( 'NONE',  ( -68.99615306438067819, 142.7668250816626596, 15.00000000000006928 ) ) ;
#15590 = EDGE_LOOP ( 'NONE', ( #11358, #13614, #5003, #10316 ) ) ;
#15591 = ORIENTED_EDGE ( 'NONE', *, *, #4310, .T. ) ;
#15592 = VECTOR ( 'NONE', #8613, 1000.000000000000114 ) ;
#15593 = AXIS2_PLACEMENT_3D ( 'NONE', #11611, #17395, #4586 ) ;
#15594 = EDGE_CURVE ( 'NONE', #15506, #10929, #8382, .T. ) ;
#15595 = FACE_OUTER_BOUND ( 'NONE', #1726, .T. ) ;
#15596 = EDGE_CURVE ( 'NONE', #12706, #800, #7752, .T. ) ;
#15597 = DIRECTION ( 'NONE',  ( 0.000000000000000000, 5.551115123125747573E-17, 1.000000000000000000 ) ) ;
#15598 = VERTEX_POINT ( 'NONE', #10569 ) ;
#15599 = CARTESIAN_POINT ( 'NONE',  ( -76.06514409945376087, 73.26749283226919829, 97.49999999999998579 ) ) ;
#15600 = LINE ( 'NONE', #2598, #16387 ) ;
#15601 = CARTESIAN_POINT ( 'NONE',  ( -50.06979403241810900, 50.58224449241409104, 26.91246033477412425 ) ) ;
#15602 = DIRECTION ( 'NONE',  ( 0.000000000000000000, -0.5000000000000017764, -0.8660254037844377084 ) ) ;
#15603 = ORIENTED_EDGE ( 'NONE', *, *, #7344, .T. ) ;
#15604 = VECTOR ( 'NONE', #6485, 1000.000000000000114 ) ;
#15605 = DIRECTION ( 'NONE',  ( -0.9396926207859022107, 0.3420201433256853663, -4.890320548438415379E-16 ) ) ;
#15606 = CARTESIAN_POINT ( 'NONE',  ( -12.84402433037575442, 28.32093258747478615, -39.79682189825760474 ) ) ;
#15607 = CARTESIAN_POINT ( 'NONE',  ( -68.99615306438076345, 99.39938383813026235, 15.00000000000006928 ) ) ;
#15608 = ORIENTED_EDGE ( 'NONE', *, *, #6372, .T. ) ;
#15609 = AXIS2_PLACEMENT_3D ( 'NONE', #16500, #13424, #515 ) ;
#15610 = AXIS2_PLACEMENT_3D ( 'NONE', #16274, #3463, #9177 ) ;
#15611 = CARTESIAN_POINT ( 'NONE',  ( -71.24615306438080609, 116.8151508545637114, -15.00000000000001421 ) ) ;
#15612 = LINE ( 'NONE', #2799, #8916 ) ;
#15613 = DIRECTION ( 'NONE',  ( 0.000000000000000000, 0.000000000000000000, 1.000000000000000000 ) ) ;
#15614 = DIRECTION ( 'NONE',  ( 0.000000000000000000, 1.000000000000000000, 0.000000000000000000 ) ) ;
#15615 = ORIENTED_EDGE ( 'NONE', *, *, #9637, .F. ) ;
#15616 = VERTEX_POINT ( 'NONE', #3742 ) ;
#15617 = AXIS2_PLACEMENT_3D ( 'NONE', #17187, #8945, #15778 ) ;
#15618 = CARTESIAN_POINT ( 'NONE',  ( -71.24615306438080609, 110.5319655545637403, -167.1454815528550739 ) ) ;
#15619 = VERTEX_POINT ( 'NONE', #13467 ) ;
#15620 = AXIS2_PLACEMENT_3D ( 'NONE', #15538, #13960, #2636 ) ;
#15621 = VECTOR ( 'NONE', #16932, 1000.000000000000114 ) ;
#15622 = CARTESIAN_POINT ( 'NONE',  ( -66.51167281958223043, 112.0421917453874556, -24.67744962832335176 ) ) ;
#15623 = DIRECTION ( 'NONE',  ( -0.7071067811864494290, 8.659560562356134638E-17, -0.7071067811866454944 ) ) ;
#15624 = CARTESIAN_POINT ( 'NONE',  ( -63.64920489524519809, -92.58099833983887095, -43.41642524957592997 ) ) ;
#15625 = VERTEX_POINT ( 'NONE', #10747 ) ;
#15626 = LINE ( 'NONE', #7112, #5965 ) ;
#15627 = CARTESIAN_POINT ( 'NONE',  ( -67.59262256747317110, 57.88796029049329661, 22.35917033480642857 ) ) ;
#15628 = LINE ( 'NONE', #14314, #9132 ) ;
#15629 = LINE ( 'NONE', #4209, #11432 ) ;
#15630 = ORIENTED_EDGE ( 'NONE', *, *, #13474, .T. ) ;
#15631 = VECTOR ( 'NONE', #789, 1000.000000000000000 ) ;
#15632 = DIRECTION ( 'NONE',  ( 0.000000000000000000, 0.000000000000000000, 1.000000000000000000 ) ) ;
#15633 = ORIENTED_EDGE ( 'NONE', *, *, #12458, .F. ) ;
#15634 = ADVANCED_FACE ( 'NONE', ( #16442 ), #3461, .T. ) ;
#15635 = AXIS2_PLACEMENT_3D ( 'NONE', #16949, #4133, #8439 ) ;
#15636 = FACE_OUTER_BOUND ( 'NONE', #16835, .T. ) ;
#15637 = CIRCLE ( 'NONE', #14141, 4.599999999999999645 ) ;
#15638 = FILL_AREA_STYLE_COLOUR ( '', #7474 ) ;
#15639 = ORIENTED_EDGE ( 'NONE', *, *, #12034, .T. ) ;
#15640 = VERTEX_POINT ( 'NONE', #9175 ) ;
#15641 = ADVANCED_FACE ( 'NONE', ( #15140 ), #651, .T. ) ;
#15642 = ORIENTED_EDGE ( 'NONE', *, *, #2492, .F. ) ;
#15643 = UNCERTAINTY_MEASURE_WITH_UNIT (LENGTH_MEASURE( 1.000000000000000082E-05 ), #12114, 'distance_accuracy_value', 'NONE');
#15644 = AXIS2_PLACEMENT_3D ( 'NONE', #8255, #10869, #11056 ) ;
#15645 = CARTESIAN_POINT ( 'NONE',  ( -68.43244712042248068, 57.12762349320347965, -22.41788552795556910 ) ) ;
#15646 = CARTESIAN_POINT ( 'NONE',  ( -68.99615306438103346, 33.42593818813029571, 15.00000000000006928 ) ) ;
#15647 = CARTESIAN_POINT ( 'NONE',  ( -78.12361985383350316, 84.22855780814607840, 70.00000000000001421 ) ) ;
#15648 = AXIS2_PLACEMENT_3D ( 'NONE', #1666, #8959, #17277 ) ;
#15649 = CARTESIAN_POINT ( 'NONE',  ( -56.41614838398844256, 95.01461175692088545, -167.1454815528550739 ) ) ;
#15650 = AXIS2_PLACEMENT_3D ( 'NONE', #9538, #13753, #6739 ) ;
#15651 = VECTOR ( 'NONE', #13739, 1000.000000000000000 ) ;
#15652 = CARTESIAN_POINT ( 'NONE',  ( -57.08002265617300708, 84.22855780814606419, -167.1454815528550739 ) ) ;
#15653 = ORIENTED_EDGE ( 'NONE', *, *, #13989, .F. ) ;
#15654 = CARTESIAN_POINT ( 'NONE',  ( -68.99615306438067819, 143.3816809381303585, -167.1454815528550739 ) ) ;
#15655 = ORIENTED_EDGE ( 'NONE', *, *, #14867, .T. ) ;
#15656 = DIRECTION ( 'NONE',  ( 0.000000000000000000, 0.000000000000000000, 1.000000000000000000 ) ) ;
#15657 = DIRECTION ( 'NONE',  ( -1.000000000000000000, 0.000000000000000000, 0.000000000000000000 ) ) ;
#15658 = ORIENTED_EDGE ( 'NONE', *, *, #7596, .T. ) ;
#15659 = DIRECTION ( 'NONE',  ( 1.000000000000000000, 0.000000000000000000, 5.551115123125780730E-16 ) ) ;
#15660 = EDGE_LOOP ( 'NONE', ( #177, #9658, #16867, #1608, #2099, #13036 ) ) ;
#15661 = VECTOR ( 'NONE', #4175, 1000.000000000000000 ) ;
#15662 = AXIS2_PLACEMENT_3D ( 'NONE', #8092, #18119, #12425 ) ;
#15663 = ORIENTED_EDGE ( 'NONE', *, *, #4795, .F. ) ;
#15664 = EDGE_CURVE ( 'NONE', #2078, #8454, #17036, .T. ) ;
#15665 = SURFACE_STYLE_USAGE ( .BOTH. , #12492 ) ;
#15666 = LINE ( 'NONE', #12863, #5197 ) ;
#15667 = CARTESIAN_POINT ( 'NONE',  ( -68.99615306438069240, 137.0984956381303164, -15.00000000000001421 ) ) ;
#15668 = EDGE_LOOP ( 'NONE', ( #3911, #9503, #3555, #8094 ) ) ;
#15669 = ORIENTED_EDGE ( 'NONE', *, *, #14454, .T. ) ;
#15670 = CARTESIAN_POINT ( 'NONE',  ( -71.24615306438103346, 46.81124181522922356, 15.00000000000006928 ) ) ;
#15671 = FACE_OUTER_BOUND ( 'NONE', #7467, .T. ) ;
#15672 = ORIENTED_EDGE ( 'NONE', *, *, #1269, .T. ) ;
#15673 = CARTESIAN_POINT ( 'NONE',  ( 93.45071565215914688, 84.22855780814606419, 74.79357405616492827 ) ) ;
#15674 = CARTESIAN_POINT ( 'NONE',  ( -68.99615306438077766, 123.9172691816626610, -15.00000000000001421 ) ) ;
#15675 = DIRECTION ( 'NONE',  ( 0.000000000000000000, 0.000000000000000000, 1.000000000000000000 ) ) ;
#15676 = CIRCLE ( 'NONE', #4886, 34.36884788726141693 ) ;
#15677 = ORIENTED_EDGE ( 'NONE', *, *, #6982, .F. ) ;
#15678 = VECTOR ( 'NONE', #13394, 1000.000000000000000 ) ;
#15679 = EDGE_CURVE ( 'NONE', #4354, #7136, #18245, .T. ) ;
#15680 = FACE_OUTER_BOUND ( 'NONE', #15352, .T. ) ;
#15681 = ORIENTED_EDGE ( 'NONE', *, *, #8192, .F. ) ;
#15682 = EDGE_CURVE ( 'NONE', #11369, #3765, #15847, .T. ) ;
#15683 = ORIENTED_EDGE ( 'NONE', *, *, #17376, .F. ) ;
#15684 =( GEOMETRIC_REPRESENTATION_CONTEXT ( 3 ) GLOBAL_UNCERTAINTY_ASSIGNED_CONTEXT ( ( #15643 ) ) GLOBAL_UNIT_ASSIGNED_CONTEXT ( ( #12114, #3862, #2093 ) ) REPRESENTATION_CONTEXT ( 'NONE', 'WORKASPACE' ) );
#15685 = DIRECTION ( 'NONE',  ( 0.000000000000000000, 1.000000000000000000, 0.000000000000000000 ) ) ;
#15686 = ORIENTED_EDGE ( 'NONE', *, *, #18437, .T. ) ;
#15687 = ORIENTED_EDGE ( 'NONE', *, *, #16175, .F. ) ;
#15688 = AXIS2_PLACEMENT_3D ( 'NONE', #7714, #18008, #9134 ) ;
#15689 = EDGE_CURVE ( 'NONE', #14192, #4281, #9351, .T. ) ;
#15690 = EDGE_CURVE ( 'NONE', #16809, #5572, #2323, .T. ) ;
#15691 = AXIS2_PLACEMENT_3D ( 'NONE', #12303, #16393, #9482 ) ;
#15692 = ADVANCED_FACE ( 'NONE', ( #8029 ), #6532, .T. ) ;
#15693 = AXIS2_PLACEMENT_3D ( 'NONE', #16438, #6237, #9251 ) ;
#15694 = DIRECTION ( 'NONE',  ( 0.000000000000000000, 0.000000000000000000, 1.000000000000000000 ) ) ;
#15695 = FACE_OUTER_BOUND ( 'NONE', #3125, .T. ) ;
#15696 = DIRECTION ( 'NONE',  ( 0.000000000000000000, 1.000000000000000000, 0.000000000000000000 ) ) ;
#15697 = ORIENTED_EDGE ( 'NONE', *, *, #2053, .F. ) ;
#15698 = DIRECTION ( 'NONE',  ( 0.000000000000000000, 0.000000000000000000, 1.000000000000000000 ) ) ;
#15699 = DIRECTION ( 'NONE',  ( 0.9396926207859084279, 0.3420201433256686574, -1.086737899652989892E-16 ) ) ;
#15700 = CARTESIAN_POINT ( 'NONE',  ( -24.42865639074866735, 38.95740195071884671, 34.21208529195362047 ) ) ;
#15701 = FACE_OUTER_BOUND ( 'NONE', #14373, .T. ) ;
#15702 = VERTEX_POINT ( 'NONE', #10845 ) ;
#15703 = EDGE_CURVE ( 'NONE', #14497, #18083, #5231, .T. ) ;
#15704 = CARTESIAN_POINT ( 'NONE',  ( -56.26901274438541378, 73.45256821284058901, 15.00000000000006928 ) ) ;
#15705 = LINE ( 'NONE', #3230, #8441 ) ;
#15706 = CARTESIAN_POINT ( 'NONE',  ( -92.59262256747321373, 110.5691553257988460, 30.35917033480641081 ) ) ;
#15707 = ORIENTED_EDGE ( 'NONE', *, *, #17726, .F. ) ;
#15708 = CIRCLE ( 'NONE', #7619, 12.49999999999999112 ) ;
#15709 = CIRCLE ( 'NONE', #3737, 9.999999999999994671 ) ;
#15710 = ADVANCED_FACE ( 'NONE', ( #11324 ), #3920, .F. ) ;
#15711 = DIRECTION ( 'NONE',  ( 0.000000000000000000, 0.000000000000000000, 1.000000000000000000 ) ) ;
#15712 = DIRECTION ( 'NONE',  ( 1.000000000000000000, 0.000000000000000000, 0.000000000000000000 ) ) ;
#15713 = EDGE_CURVE ( 'NONE', #1208, #14302, #18149, .T. ) ;
#15714 = FACE_OUTER_BOUND ( 'NONE', #18062, .T. ) ;
#15715 = DIRECTION ( 'NONE',  ( -5.204170427930409450E-16, 0.000000000000000000, 1.000000000000000000 ) ) ;
#15716 = ORIENTED_EDGE ( 'NONE', *, *, #6156, .T. ) ;
#15717 = ORIENTED_EDGE ( 'NONE', *, *, #5847, .T. ) ;
#15718 = EDGE_CURVE ( 'NONE', #14794, #14048, #5317, .T. ) ;
#15719 = DIRECTION ( 'NONE',  ( -2.062304371594500494E-16, 1.000000000000000000, -0.000000000000000000 ) ) ;
#15720 = VERTEX_POINT ( 'NONE', #9632 ) ;
#15721 = AXIS2_PLACEMENT_3D ( 'NONE', #4849, #3184, #650 ) ;
#15722 = VECTOR ( 'NONE', #11771, 1000.000000000000000 ) ;
#15723 = FACE_OUTER_BOUND ( 'NONE', #11336, .T. ) ;
#15724 = FACE_OUTER_BOUND ( 'NONE', #8903, .T. ) ;
#15725 = ORIENTED_EDGE ( 'NONE', *, *, #10694, .F. ) ;
#15726 = CARTESIAN_POINT ( 'NONE',  ( -71.24615306438100504, 53.98329785456373742, 15.00000000000006928 ) ) ;
#15727 = CARTESIAN_POINT ( 'NONE',  ( -59.35080917176598092, 94.79374675277695417, -167.1454815528550739 ) ) ;
#15728 = CARTESIAN_POINT ( 'NONE',  ( 45.30000000000000426, 1.912636715672988680E-16, 3.445500000000021767 ) ) ;
#15729 = EDGE_LOOP ( 'NONE', ( #12223, #2370, #13421, #17560 ) ) ;
#15730 = DIRECTION ( 'NONE',  ( 0.000000000000000000, 1.000000000000000000, 0.000000000000000000 ) ) ;
#15731 = CARTESIAN_POINT ( 'NONE',  ( -71.24615306438080609, 107.3903729045637192, -167.1454815528550739 ) ) ;
#15732 = ORIENTED_EDGE ( 'NONE', *, *, #7982, .F. ) ;
#15733 = CARTESIAN_POINT ( 'NONE',  ( -47.80867013224673912, 89.78028827820993740, -167.1454815528550739 ) ) ;
#15734 = CARTESIAN_POINT ( 'NONE',  ( -68.99615306438111872, 13.96152643166267993, 15.00000000000006928 ) ) ;
#15735 = ORIENTED_EDGE ( 'NONE', *, *, #1275, .T. ) ;
#15736 = EDGE_LOOP ( 'NONE', ( #3018, #6588, #3607, #3535 ) ) ;
#15737 = LINE ( 'NONE', #2919, #2848 ) ;
#15738 = DIRECTION ( 'NONE',  ( 0.000000000000000000, 0.000000000000000000, 1.000000000000000000 ) ) ;
#15739 = PLANE ( 'NONE',  #8641 ) ;
#15740 = CARTESIAN_POINT ( 'NONE',  ( 15.23320273812467462, -111.0842361345572158, -57.00000000000000000 ) ) ;
#15741 = CARTESIAN_POINT ( 'NONE',  ( -56.59294758719027385, 94.46597735006069740, -15.00000000000001421 ) ) ;
#15742 = ORIENTED_EDGE ( 'NONE', *, *, #13616, .F. ) ;
#15743 = DIRECTION ( 'NONE',  ( 0.3420201433256686574, 0.9396926207859084279, -0.000000000000000000 ) ) ;
#15744 = VERTEX_POINT ( 'NONE', #15338 ) ;
#15745 = DIRECTION ( 'NONE',  ( 0.000000000000000000, 0.000000000000000000, 1.000000000000000000 ) ) ;
#15746 = LINE ( 'NONE', #4412, #9565 ) ;
#15747 = EDGE_LOOP ( 'NONE', ( #15811, #8744, #7117, #17576 ) ) ;
#15748 = DIRECTION ( 'NONE',  ( 1.000000000000000000, 0.000000000000000000, 3.771137991253934490E-16 ) ) ;
#15749 = ORIENTED_EDGE ( 'NONE', *, *, #8914, .T. ) ;
#15750 = VERTEX_POINT ( 'NONE', #15726 ) ;
#15751 = DIRECTION ( 'NONE',  ( 1.000000000000000000, 0.000000000000000000, 0.000000000000000000 ) ) ;
#15752 = CARTESIAN_POINT ( 'NONE',  ( -107.5926225674732137, 117.8748711238780373, -25.00000000000000000 ) ) ;
#15753 = CARTESIAN_POINT ( 'NONE',  ( 56.85086857400936822, 84.22855780814606419, 62.50000000000001421 ) ) ;
#15754 = ORIENTED_EDGE ( 'NONE', *, *, #871, .T. ) ;
#15755 = ITEM_DEFINED_TRANSFORMATION ( 'NONE', 'NONE', #1327,  #16217 ) ;
#15756 = DIRECTION ( 'NONE',  ( 0.000000000000000000, 0.000000000000000000, 1.000000000000000000 ) ) ;
#15757 = EDGE_LOOP ( 'NONE', ( #4370, #923, #16626, #7157 ) ) ;
#15758 = DIRECTION ( 'NONE',  ( -1.000000000000000000, 1.099120794378904723E-13, 1.387778780781445182E-16 ) ) ;
#15759 = DIRECTION ( 'NONE',  ( 1.000000000000000000, 0.000000000000000000, -0.000000000000000000 ) ) ;
#15760 = CARTESIAN_POINT ( 'NONE',  ( -70.85175816390371040, -141.5628872026273086, -57.00000000000000000 ) ) ;
#15761 = ORIENTED_EDGE ( 'NONE', *, *, #8372, .T. ) ;
#15762 = DIRECTION ( 'NONE',  ( -0.000000000000000000, -0.000000000000000000, -1.000000000000000000 ) ) ;
#15763 = VERTEX_POINT ( 'NONE', #11036 ) ;
#15764 = EDGE_CURVE ( 'NONE', #7124, #9028, #17866, .T. ) ;
#15765 = ORIENTED_EDGE ( 'NONE', *, *, #14433, .T. ) ;
#15766 = LINE ( 'NONE', #2950, #1630 ) ;
#15767 = ORIENTED_EDGE ( 'NONE', *, *, #5612, .F. ) ;
#15768 = CARTESIAN_POINT ( 'NONE',  ( -57.08002265617300708, 84.22855780814606419, -167.1454815528550739 ) ) ;
#15769 = EDGE_CURVE ( 'NONE', #9327, #14302, #2906, .T. ) ;
#15770 = LINE ( 'NONE', #4437, #6357 ) ;
#15771 = ORIENTED_EDGE ( 'NONE', *, *, #9396, .F. ) ;
#15772 = CARTESIAN_POINT ( 'NONE',  ( -57.08002265617300708, 84.22855780814606419, 15.00000000000006928 ) ) ;
#15773 = DIRECTION ( 'NONE',  ( -1.000000000000000000, 0.000000000000000000, 0.000000000000000000 ) ) ;
#15774 = CARTESIAN_POINT ( 'NONE',  ( -68.99615306438076345, 111.9657544381302330, -15.00000000000001421 ) ) ;
#15775 = DIRECTION ( 'NONE',  ( -0.000000000000000000, -0.000000000000000000, -1.000000000000000000 ) ) ;
#15776 = ORIENTED_EDGE ( 'NONE', *, *, #3554, .T. ) ;
#15777 = FACE_OUTER_BOUND ( 'NONE', #3417, .T. ) ;
#15778 = DIRECTION ( 'NONE',  ( 1.000000000000000000, 0.000000000000000000, 5.204170427930409450E-16 ) ) ;
#15779 = LINE ( 'NONE', #4374, #16176 ) ;
#15780 = ORIENTED_EDGE ( 'NONE', *, *, #15087, .F. ) ;
#15781 = EDGE_CURVE ( 'NONE', #6312, #10938, #13943, .T. ) ;
#15782 = EDGE_CURVE ( 'NONE', #7810, #5163, #6919, .T. ) ;
#15783 = CARTESIAN_POINT ( 'NONE',  ( -66.39376235201207521, 88.50596986196454452, -167.1454815528550739 ) ) ;
#15784 = AXIS2_PLACEMENT_3D ( 'NONE', #1354, #13120, #5984 ) ;
#15785 = DIRECTION ( 'NONE',  ( 1.000000000000000000, 0.000000000000000000, -0.000000000000000000 ) ) ;
#15786 = CYLINDRICAL_SURFACE ( 'NONE', #2401, 12.49999999999999112 ) ;
#15787 = VERTEX_POINT ( 'NONE', #12820 ) ;
#15788 = ORIENTED_EDGE ( 'NONE', *, *, #17249, .F. ) ;
#15789 = EDGE_CURVE ( 'NONE', #7618, #2809, #9566, .T. ) ;
#15790 = EDGE_CURVE ( 'NONE', #17935, #9354, #7188, .T. ) ;
#15791 = CARTESIAN_POINT ( 'NONE',  ( -71.24615306438100504, 53.98329785456373742, -15.00000000000001421 ) ) ;
#15792 = DIRECTION ( 'NONE',  ( 1.000000000000000000, 0.000000000000000000, 0.000000000000000000 ) ) ;
#15793 = FACE_OUTER_BOUND ( 'NONE', #17179, .T. ) ;
#15794 = DIRECTION ( 'NONE',  ( 0.000000000000000000, 0.000000000000000000, 1.000000000000000000 ) ) ;
#15795 = EDGE_CURVE ( 'NONE', #4091, #6648, #1322, .T. ) ;
#15796 = VECTOR ( 'NONE', #11428, 1000.000000000000000 ) ;
#15797 = DIRECTION ( 'NONE',  ( 0.000000000000000000, 1.000000000000000000, 0.000000000000000000 ) ) ;
#15798 = ORIENTED_EDGE ( 'NONE', *, *, #11687, .F. ) ;
#15799 = CARTESIAN_POINT ( 'NONE',  ( 44.74549999999999272, 0.000000000000000000, 0.000000000000000000 ) ) ;
#15800 = LINE ( 'NONE', #15627, #11543 ) ;
#15801 = DIRECTION ( 'NONE',  ( 1.000000000000000000, 0.000000000000000000, 0.000000000000000000 ) ) ;
#15802 = FACE_OUTER_BOUND ( 'NONE', #341, .T. ) ;
#15803 = ORIENTED_EDGE ( 'NONE', *, *, #6478, .F. ) ;
#15804 = CARTESIAN_POINT ( 'NONE',  ( -37.06257812395524098, 90.72084218871721362, 66.26299256513551938 ) ) ;
#15805 = EDGE_CURVE ( 'NONE', #4264, #15435, #5383, .T. ) ;
#15806 = EDGE_CURVE ( 'NONE', #17762, #3055, #16987, .T. ) ;
#15807 = LINE ( 'NONE', #1330, #599 ) ;
#15808 = VERTEX_POINT ( 'NONE', #12750 ) ;
#15809 = DIRECTION ( 'NONE',  ( 0.000000000000000000, 0.000000000000000000, -1.000000000000000000 ) ) ;
#15810 = DIRECTION ( 'NONE',  ( 0.000000000000000000, 0.000000000000000000, 1.000000000000000000 ) ) ;
#15811 = ORIENTED_EDGE ( 'NONE', *, *, #14812, .T. ) ;
#15812 = CIRCLE ( 'NONE', #7438, 4.600000000000006750 ) ;
#15813 = VERTEX_POINT ( 'NONE', #5602 ) ;
#15814 = EDGE_LOOP ( 'NONE', ( #3343, #17696, #17758, #3385 ) ) ;
#15815 = DIRECTION ( 'NONE',  ( -0.9396926207859093161, 0.3420201433256661594, 1.086737899652990878E-16 ) ) ;
#15816 = CARTESIAN_POINT ( 'NONE',  ( -46.69442755757756203, 81.24207102880484399, 15.00000000000009592 ) ) ;
#15817 = EDGE_CURVE ( 'NONE', #11585, #17119, #15626, .T. ) ;
#15818 = CARTESIAN_POINT ( 'NONE',  ( -57.08002265617300708, 84.22855780814606419, -61.50000000000001421 ) ) ;
#15819 = LINE ( 'NONE', #17567, #7469 ) ;
#15820 = CARTESIAN_POINT ( 'NONE',  ( -57.08002265617300708, 84.22855780814606419, -124.8487082408420861 ) ) ;
#15821 = VERTEX_POINT ( 'NONE', #17111 ) ;
#15822 = CIRCLE ( 'NONE', #2070, 21.04359719766050318 ) ;
#15823 = LINE ( 'NONE', #15462, #13491 ) ;
#15824 = ORIENTED_EDGE ( 'NONE', *, *, #10197, .F. ) ;
#15825 = CARTESIAN_POINT ( 'NONE',  ( -78.02975850117555012, -92.35432678654406402, 43.13417664947079544 ) ) ;
#15826 = AXIS2_PLACEMENT_3D ( 'NONE', #5864, #7539, #15785 ) ;
#15827 = DIRECTION ( 'NONE',  ( 1.000000000000000000, 0.000000000000000000, 3.771137991253923150E-16 ) ) ;
#15828 = EDGE_LOOP ( 'NONE', ( #1822, #7068, #6324, #5865 ) ) ;
#15829 = CARTESIAN_POINT ( 'NONE',  ( 15.23320273812466574, -111.0842361345572158, 57.00000000000000000 ) ) ;
#15830 = ORIENTED_EDGE ( 'NONE', *, *, #11316, .F. ) ;
#15831 = AXIS2_PLACEMENT_3D ( 'NONE', #5633, #11355, #15657 ) ;
#15832 = ORIENTED_EDGE ( 'NONE', *, *, #10520, .F. ) ;
#15833 = VECTOR ( 'NONE', #1427, 1000.000000000000000 ) ;
#15834 = CARTESIAN_POINT ( 'NONE',  ( -47.19781944808393348, 88.60139997190906058, 15.00000000000009592 ) ) ;
#15835 = DIRECTION ( 'NONE',  ( 1.000000000000000000, 0.000000000000000000, 0.000000000000000000 ) ) ;
#15836 = DIRECTION ( 'NONE',  ( 0.000000000000000000, 0.000000000000000000, -1.000000000000000000 ) ) ;
#15837 = VERTEX_POINT ( 'NONE', #5785 ) ;
#15838 = ORIENTED_EDGE ( 'NONE', *, *, #587, .T. ) ;
#15839 = LINE ( 'NONE', #9870, #4792 ) ;
#15840 = CARTESIAN_POINT ( 'NONE',  ( -71.24615306438080609, 109.6430948152292189, -15.00000000000001421 ) ) ;
#15841 = CARTESIAN_POINT ( 'NONE',  ( -36.44155368744862500, 56.74635804676027107, 2.999999999999999112 ) ) ;
#15842 = DIRECTION ( 'NONE',  ( -1.000000000000000000, 0.000000000000000000, 0.000000000000000000 ) ) ;
#15843 = ORIENTED_EDGE ( 'NONE', *, *, #5376, .T. ) ;
#15844 = AXIS2_PLACEMENT_3D ( 'NONE', #6326, #2035, #6137 ) ;
#15845 = CARTESIAN_POINT ( 'NONE',  ( -70.71978124295708312, -96.08423613455721579, 22.52877280353970235 ) ) ;
#15846 = EDGE_LOOP ( 'NONE', ( #3279, #7397, #16186, #10217, #6073, #9909, #2570 ) ) ;
#15847 = CIRCLE ( 'NONE', #604, 11.04359719766050141 ) ;
#15848 = ORIENTED_EDGE ( 'NONE', *, *, #255, .T. ) ;
#15849 = VECTOR ( 'NONE', #5773, 1000.000000000000000 ) ;
#15850 = EDGE_CURVE ( 'NONE', #11731, #9165, #10366, .T. ) ;
#15851 = ORIENTED_EDGE ( 'NONE', *, *, #6750, .F. ) ;
#15852=STYLED_ITEM('',(#18545),#6144);
#15853 = DIRECTION ( 'NONE',  ( -2.062304371594500494E-16, 1.000000000000000000, -0.000000000000000000 ) ) ;
#15854 = CYLINDRICAL_SURFACE ( 'NONE', #6689, 3.999999999999996447 ) ;
#15855 = FACE_OUTER_BOUND ( 'NONE', #30, .T. ) ;
#15856 = ORIENTED_EDGE ( 'NONE', *, *, #17965, .F. ) ;
#15857 = AXIS2_PLACEMENT_3D ( 'NONE', #9800, #16802, #14111 ) ;
#15858 = DIRECTION ( 'NONE',  ( 0.000000000000000000, 0.000000000000000000, 1.000000000000000000 ) ) ;
#15859 = CARTESIAN_POINT ( 'NONE',  ( -71.24615306438091977, 78.22716831522920700, 15.00000000000006928 ) ) ;
#15860 = CARTESIAN_POINT ( 'NONE',  ( -71.24615306438080609, 106.5015021652292404, -15.00000000000001421 ) ) ;
#15861 = DIRECTION ( 'NONE',  ( 1.000000000000000000, 0.000000000000000000, 0.000000000000000000 ) ) ;
#15862 = VERTEX_POINT ( 'NONE', #13093 ) ;
#15863 = CARTESIAN_POINT ( 'NONE',  ( -46.27380910617147691, 84.15481808402802244, -167.1454815528550739 ) ) ;
#15864 = LINE ( 'NONE', #14472, #2770 ) ;
#15865 = CARTESIAN_POINT ( 'NONE',  ( -97.59262256747318531, 57.88796029049330372, 26.35917033480641436 ) ) ;
#15866 = ORIENTED_EDGE ( 'NONE', *, *, #9492, .T. ) ;
#15867 = CIRCLE ( 'NONE', #10780, 11.04359719766049430 ) ;
#15868 = LINE ( 'NONE', #1566, #2845 ) ;
#15869 = CARTESIAN_POINT ( 'NONE',  ( -53.97067643794850511, 72.12145385653101926, 15.00000000000006928 ) ) ;
#15870 = AXIS2_PLACEMENT_3D ( 'NONE', #16395, #14902, #705 ) ;
#15871 = AXIS2_PLACEMENT_3D ( 'NONE', #14010, #12619, #4368 ) ;
#15872 = ORIENTED_EDGE ( 'NONE', *, *, #3512, .F. ) ;
#15873 = ORIENTED_EDGE ( 'NONE', *, *, #12121, .T. ) ;
#15874 = ADVANCED_FACE ( 'NONE', ( #11857 ), #6131, .T. ) ;
#15875 = DIRECTION ( 'NONE',  ( 1.000000000000000000, 0.000000000000000000, 0.000000000000000000 ) ) ;
#15876 = VECTOR ( 'NONE', #12674, 1000.000000000000000 ) ;
#15877 = EDGE_CURVE ( 'NONE', #3544, #7512, #8692, .T. ) ;
#15878 = CARTESIAN_POINT ( 'NONE',  ( -57.08002265617300708, 84.22855780814606419, 15.00000000000006928 ) ) ;
#15879 = DIRECTION ( 'NONE',  ( 0.3420201433256686574, -0.9396926207859084279, 0.000000000000000000 ) ) ;
#15880 = EDGE_LOOP ( 'NONE', ( #2262, #1421, #2417, #5606 ) ) ;
#15881 = DIRECTION ( 'NONE',  ( 0.9396926207859110924, 0.3420201433256611634, 0.000000000000000000 ) ) ;
#15882 = AXIS2_PLACEMENT_3D ( 'NONE', #17162, #8648, #1632 ) ;
#15883 = PLANE ( 'NONE',  #12423 ) ;
#15884 = DIRECTION ( 'NONE',  ( 0.000000000000000000, 0.5000000000000017764, 0.8660254037844375974 ) ) ;
#15885 = FACE_OUTER_BOUND ( 'NONE', #13128, .T. ) ;
#15886 = ORIENTED_EDGE ( 'NONE', *, *, #6210, .F. ) ;
#15887 = CARTESIAN_POINT ( 'NONE',  ( -36.17234154033610594, 86.65978693925961807, 69.61194856958498178 ) ) ;
#15888 = EDGE_CURVE ( 'NONE', #9582, #7975, #12887, .T. ) ;
#15889 = CARTESIAN_POINT ( 'NONE',  ( -71.24615306438084872, 75.97444640456379261, 15.00000000000006928 ) ) ;
#15890 = EDGE_CURVE ( 'NONE', #11331, #16706, #1223, .T. ) ;
#15891 = ORIENTED_EDGE ( 'NONE', *, *, #9268, .T. ) ;
#15892 = ADVANCED_FACE ( 'NONE', ( #16144 ), #17546, .T. ) ;
#15893 = VECTOR ( 'NONE', #17531, 1000.000000000000000 ) ;
#15894 = CARTESIAN_POINT ( 'NONE',  ( -68.99615306438094819, 52.27549408813023746, -167.1454815528550739 ) ) ;
#15895 = DIRECTION ( 'NONE',  ( 1.156482317317869999E-16, 0.000000000000000000, 1.000000000000000000 ) ) ;
#15896 = VERTEX_POINT ( 'NONE', #3333 ) ;
#15897 = ORIENTED_EDGE ( 'NONE', *, *, #3135, .T. ) ;
#15898 = AXIS2_PLACEMENT_3D ( 'NONE', #17834, #7734, #3613 ) ;
#15899 = VECTOR ( 'NONE', #18242, 1000.000000000000000 ) ;
#15900 = EDGE_CURVE ( 'NONE', #1479, #14497, #14947, .T. ) ;
#15901 = ORIENTED_EDGE ( 'NONE', *, *, #13628, .F. ) ;
#15902 = EDGE_CURVE ( 'NONE', #10995, #5674, #7555, .T. ) ;
#15903 = ADVANCED_FACE ( 'NONE', ( #14572 ), #264, .T. ) ;
#15904 = DIRECTION ( 'NONE',  ( 0.000000000000000000, 0.000000000000000000, -1.000000000000000000 ) ) ;
#15905 = CARTESIAN_POINT ( 'NONE',  ( 0.5805565836007609004, -3.752776749732685158, 6.500000000000043521 ) ) ;
#15906 = CARTESIAN_POINT ( 'NONE',  ( -71.24615306438111872, 18.53690796522925055, -15.00000000000001421 ) ) ;
#15907 = CIRCLE ( 'NONE', #1570, 3.999999999999989786 ) ;
#15908 = ADVANCED_FACE ( 'NONE', ( #9058 ), #7197, .F. ) ;
#15909 = DIRECTION ( 'NONE',  ( 0.000000000000000000, 0.000000000000000000, 1.000000000000000000 ) ) ;
#15910 = DIRECTION ( 'NONE',  ( -0.000000000000000000, -0.000000000000000000, -1.000000000000000000 ) ) ;
#15911 = VERTEX_POINT ( 'NONE', #8965 ) ;
#15912 = EDGE_CURVE ( 'NONE', #8070, #9559, #5954, .T. ) ;
#15913 = DIRECTION ( 'NONE',  ( 1.000000000000000000, 0.000000000000000000, 3.771137991253928573E-16 ) ) ;
#15914 = CARTESIAN_POINT ( 'NONE',  ( -57.08002265617300708, 84.22855780814606419, -61.50000000000000000 ) ) ;
#15915 = AXIS2_PLACEMENT_3D ( 'NONE', #884, #6691, #8188 ) ;
#15916 = VECTOR ( 'NONE', #8846, 1000.000000000000114 ) ;
#15917 = LINE ( 'NONE', #3107, #7185 ) ;
#15918 = ORIENTED_EDGE ( 'NONE', *, *, #9852, .F. ) ;
#15919 = CARTESIAN_POINT ( 'NONE',  ( -71.24615306438080609, 104.2487802545637408, -167.1454815528550739 ) ) ;
#15920 = DIRECTION ( 'NONE',  ( 0.000000000000000000, 0.000000000000000000, -1.000000000000000000 ) ) ;
#15921 = EDGE_CURVE ( 'NONE', #5963, #10059, #7205, .T. ) ;
#15922 = EDGE_LOOP ( 'NONE', ( #6636, #7720, #17310, #12255 ) ) ;
#15923 = EDGE_CURVE ( 'NONE', #11331, #9602, #6908, .T. ) ;
#15924 = VECTOR ( 'NONE', #14969, 1000.000000000000000 ) ;
#15925 = ORIENTED_EDGE ( 'NONE', *, *, #4109, .T. ) ;
#15926 = VECTOR ( 'NONE', #14419, 1000.000000000000000 ) ;
#15927 = AXIS2_PLACEMENT_3D ( 'NONE', #12483, #15372, #17042 ) ;
#15928 = VECTOR ( 'NONE', #6525, 1000.000000000000000 ) ;
#15929 = DIRECTION ( 'NONE',  ( 0.9396926207859084279, 0.3420201433256686574, 4.890320548438448905E-16 ) ) ;
#15930 = DIRECTION ( 'NONE',  ( 0.9396926207859064295, 0.3420201433256737089, -1.086737899652987550E-16 ) ) ;
#15931 = DIRECTION ( 'NONE',  ( 1.000000000000000000, 0.000000000000000000, 0.000000000000000000 ) ) ;
#15932 = VERTEX_POINT ( 'NONE', #8788 ) ;
#15933 = ORIENTED_EDGE ( 'NONE', *, *, #10085, .T. ) ;
#15934 = CARTESIAN_POINT ( 'NONE',  ( -71.24615306438080609, 104.2487802545637408, -167.1454815528550739 ) ) ;
#15935 = CARTESIAN_POINT ( 'NONE',  ( -68.99615306438076345, 124.5321250381302747, -15.00000000000001421 ) ) ;
#15936 = CARTESIAN_POINT ( 'NONE',  ( -68.99615306438072082, 133.3420471316626958, -15.00000000000001421 ) ) ;
#15937 = DIRECTION ( 'NONE',  ( -1.000000000000000000, -0.000000000000000000, -0.000000000000000000 ) ) ;
#15938 = ORIENTED_EDGE ( 'NONE', *, *, #5939, .F. ) ;
#15939 = DIRECTION ( 'NONE',  ( 1.000000000000000000, 2.062304371594500740E-16, 0.000000000000000000 ) ) ;
#15940 = ORIENTED_EDGE ( 'NONE', *, *, #1968, .F. ) ;
#15941 = VECTOR ( 'NONE', #10069, 1000.000000000000000 ) ;
#15943 = ORIENTED_EDGE ( 'NONE', *, *, #8487, .F. ) ;
#15942 = AXIS2_PLACEMENT_3D ( 'NONE', #2360, #8068, #5455 ) ;
#15944 = VERTEX_POINT ( 'NONE', #4556 ) ;
#15945 = CLOSED_SHELL ( 'NONE', ( #12224, #12493, #7896, #13645, #13728, #15450, #4273, #10979, #3076, #14190, #12486, #11290, #14164, #7331, #6884, #16509, #5710, #5166, #1159, #4056, #7125, #8104, #4912, #3556, #12550, #9261, #6997, #18417, #16202 ) ) ;
#15946 = DIRECTION ( 'NONE',  ( -1.000000000000000000, -0.000000000000000000, -0.000000000000000000 ) ) ;
#15947 = DIRECTION ( 'NONE',  ( 1.000000000000000000, 0.000000000000000000, 0.000000000000000000 ) ) ;
#15948 = VERTEX_POINT ( 'NONE', #4467 ) ;
#15949 = VECTOR ( 'NONE', #16241, 1000.000000000000000 ) ;
#15950 = CARTESIAN_POINT ( 'NONE',  ( -68.99615306438070661, 136.4836397816626743, -167.1454815528550739 ) ) ;
#15952 = CIRCLE ( 'NONE', #10130, 42.49926016645017057 ) ;
#15951 = CARTESIAN_POINT ( 'NONE',  ( -71.24615306438076345, 122.2094654152292037, -167.1454815528550739 ) ) ;
#15953 = CARTESIAN_POINT ( 'NONE',  ( -69.37109144396066540, 81.95267818613797317, 15.00000000000006928 ) ) ;
#15954 = DIRECTION ( 'NONE',  ( 0.9396926207859097602, 0.3420201433256649381, 4.890320548438455808E-16 ) ) ;
#15955 = VERTEX_POINT ( 'NONE', #14491 ) ;
#15956 = ADVANCED_FACE ( 'NONE', ( #7378 ), #10274, .T. ) ;
#15957 = CARTESIAN_POINT ( 'NONE',  ( -68.99615306438111872, 7.678341131662685726, -15.00000000000001421 ) ) ;
#15958 = DIRECTION ( 'NONE',  ( -0.000000000000000000, -1.000000000000000000, 0.000000000000000000 ) ) ;
#15959 = DIRECTION ( 'NONE',  ( 1.156482317317869999E-16, 0.000000000000000000, 1.000000000000000000 ) ) ;
#15960 = EDGE_LOOP ( 'NONE', ( #11779, #16688, #13166, #40 ) ) ;
#15961 = CIRCLE ( 'NONE', #1926, 9.999999999999994671 ) ;
#15962 = DIRECTION ( 'NONE',  ( 0.000000000000000000, 0.000000000000000000, 1.000000000000000000 ) ) ;
#15963 = VECTOR ( 'NONE', #18031, 999.9999999999998863 ) ;
#15964 = CARTESIAN_POINT ( 'NONE',  ( -67.00421887699711476, 86.78830982163884755, -167.1454815528550739 ) ) ;
#15965 = VECTOR ( 'NONE', #15954, 1000.000000000000114 ) ;
#15966 = ORIENTED_EDGE ( 'NONE', *, *, #17173, .F. ) ;
#15967 = AXIS2_PLACEMENT_3D ( 'NONE', #3937, #9756, #2553 ) ;
#15968 = VERTEX_POINT ( 'NONE', #13269 ) ;
#15969 = ORIENTED_EDGE ( 'NONE', *, *, #17580, .T. ) ;
#15970 = CARTESIAN_POINT ( 'NONE',  ( -57.08002265617300708, 84.22855780814606419, -62.50000000000000000 ) ) ;
#15971 = VECTOR ( 'NONE', #3119, 1000.000000000000000 ) ;
#15972 = DIRECTION ( 'NONE',  ( -1.000000000000000000, -0.000000000000000000, -0.000000000000000000 ) ) ;
#15973 = DIRECTION ( 'NONE',  ( -0.5150380749100570421, 0.000000000000000000, 0.8571673007021106683 ) ) ;
#15974 = DIRECTION ( 'NONE',  ( 1.000000000000000000, 0.000000000000000000, 0.000000000000000000 ) ) ;
#15975 = ORIENTED_EDGE ( 'NONE', *, *, #15560, .F. ) ;
#15976 = AXIS2_PLACEMENT_3D ( 'NONE', #14908, #17625, #16223 ) ;
#15977 = DIRECTION ( 'NONE',  ( 0.000000000000000000, 0.000000000000000000, 1.000000000000000000 ) ) ;
#15978 = VECTOR ( 'NONE', #2529, 1000.000000000000114 ) ;
#15979 = CARTESIAN_POINT ( 'NONE',  ( 4.699999999999995737, 0.000000000000000000, 0.000000000000000000 ) ) ;
#15980 = DIRECTION ( 'NONE',  ( -0.7071067811864494290, 8.659560562356134638E-17, -0.7071067811866454944 ) ) ;
#15981 = VECTOR ( 'NONE', #8126, 1000.000000000000000 ) ;
#15982 = CARTESIAN_POINT ( 'NONE',  ( -46.65463807863145007, 87.07303407725225952, -167.1454815528550739 ) ) ;
#15983 = CARTESIAN_POINT ( 'NONE',  ( -37.13915117359674412, 90.95236025322212470, 59.16826207617363309 ) ) ;
#15984 = LINE ( 'NONE', #4836, #1222 ) ;
#15985 = VERTEX_POINT ( 'NONE', #6043 ) ;
#15986 = EDGE_CURVE ( 'NONE', #1839, #4587, #1848, .T. ) ;
#15987 = CARTESIAN_POINT ( 'NONE',  ( -71.24615306438083451, 97.07672421522921979, 15.00000000000006928 ) ) ;
#15988 = VERTEX_POINT ( 'NONE', #16419 ) ;
#15989 = VERTEX_POINT ( 'NONE', #6606 ) ;
#15990 = AXIS2_PLACEMENT_3D ( 'NONE', #10758, #3750, #13856 ) ;
#15991 = CIRCLE ( 'NONE', #4062, 10.24900000000000055 ) ;
#15992 = AXIS2_PLACEMENT_3D ( 'NONE', #17207, #4391, #10099 ) ;
#15993 = VERTEX_POINT ( 'NONE', #12145 ) ;
#15994 = CARTESIAN_POINT ( 'NONE',  ( 0.5805565836007609004, 3.752776749732435135, 6.499999999999981348 ) ) ;
#15995 = DIRECTION ( 'NONE',  ( -0.9396926207859103153, 0.3420201433256635504, 1.086737899652991987E-16 ) ) ;
#15996 = ADVANCED_FACE ( 'NONE', ( #3808 ), #3610, .T. ) ;
#15997 = CARTESIAN_POINT ( 'NONE',  ( -50.41499038512539954, 117.9449492212793444, 7.000000000000010658 ) ) ;
#15998 = LINE ( 'NONE', #13466, #16555 ) ;
#15999 = EDGE_CURVE ( 'NONE', #16487, #4375, #9232, .T. ) ;
#16000 = FACE_OUTER_BOUND ( 'NONE', #6413, .T. ) ;
#16001 = DIRECTION ( 'NONE',  ( -1.000000000000000000, -0.000000000000000000, -0.000000000000000000 ) ) ;
#16002 = VERTEX_POINT ( 'NONE', #2026 ) ;
#16003 = DIRECTION ( 'NONE',  ( -5.204170427930409450E-16, 0.000000000000000000, 1.000000000000000000 ) ) ;
#16004 = FACE_OUTER_BOUND ( 'NONE', #842, .T. ) ;
#16005 = CARTESIAN_POINT ( 'NONE',  ( -68.99615306438100504, 39.70912348813028103, -15.00000000000001421 ) ) ;
#16006 = ORIENTED_EDGE ( 'NONE', *, *, #15324, .F. ) ;
#16007 = EDGE_CURVE ( 'NONE', #7696, #13982, #14922, .T. ) ;
#16008 = EDGE_CURVE ( 'NONE', #535, #9559, #15025, .T. ) ;
#16009 = CARTESIAN_POINT ( 'NONE',  ( -47.76628296033400289, 88.50596986196467242, 15.00000000000006928 ) ) ;
#16010 = FACE_OUTER_BOUND ( 'NONE', #2877, .T. ) ;
#16011 = VERTEX_POINT ( 'NONE', #5106 ) ;
#16012 = VERTEX_POINT ( 'NONE', #10822 ) ;
#16013 = ADVANCED_FACE ( 'NONE', ( #12048, #16520, #1944, #904, #3718, #6221 ), #2216, .F. ) ;
#16014 = CARTESIAN_POINT ( 'NONE',  ( -57.08002265617300708, 84.22855780814606419, 92.50000000000000000 ) ) ;
#16015 = EDGE_CURVE ( 'NONE', #9102, #8996, #17746, .T. ) ;
#16016 = DIRECTION ( 'NONE',  ( 1.156482317317869999E-16, 0.000000000000000000, 1.000000000000000000 ) ) ;
#16017 = DIRECTION ( 'NONE',  ( -1.000000000000000000, 0.000000000000000000, 0.000000000000000000 ) ) ;
#16018 = ORIENTED_EDGE ( 'NONE', *, *, #4027, .T. ) ;
#16019 = ADVANCED_FACE ( 'NONE', ( #4930 ), #6317, .T. ) ;
#16020 = EDGE_CURVE ( 'NONE', #293, #4298, #10187, .T. ) ;
#16021 = ORIENTED_EDGE ( 'NONE', *, *, #12737, .F. ) ;
#16022 = CARTESIAN_POINT ( 'NONE',  ( 5.299999999999996270, 7.830936570423732126E-16, 4.400000000000027889 ) ) ;
#16023 = CARTESIAN_POINT ( 'NONE',  ( -106.3193689061042164, 112.6569076202650450, 102.5000000000000000 ) ) ;
#16024 = DIRECTION ( 'NONE',  ( 0.000000000000000000, 0.000000000000000000, 1.000000000000000000 ) ) ;
#16025 = CARTESIAN_POINT ( 'NONE',  ( -70.71978124295696944, -91.08423613455721579, 5.204170427930421283E-15 ) ) ;
#16026 = ORIENTED_EDGE ( 'NONE', *, *, #17728, .T. ) ;
#16027 = DIRECTION ( 'NONE',  ( 1.000000000000000000, 0.000000000000000000, 5.077734830647295768E-16 ) ) ;
#16028 = ORIENTED_EDGE ( 'NONE', *, *, #4981, .T. ) ;
#16029 = EDGE_CURVE ( 'NONE', #14653, #10695, #13640, .T. ) ;
#16030 = CARTESIAN_POINT ( 'NONE',  ( -68.99615306438070661, 136.4836397816626743, 15.00000000000006928 ) ) ;
#16031 = ORIENTED_EDGE ( 'NONE', *, *, #16836, .F. ) ;
#16032 = VERTEX_POINT ( 'NONE', #5208 ) ;
#16033 = DIRECTION ( 'NONE',  ( 0.000000000000000000, -0.5000000000000008882, 0.8660254037844381525 ) ) ;
#16034 = CARTESIAN_POINT ( 'NONE',  ( 4.699999999999995737, -5.629165124598996428, -3.250000000000020428 ) ) ;
#16035 = EDGE_LOOP ( 'NONE', ( #8585, #776, #2290, #11868 ) ) ;
#16036 = FACE_OUTER_BOUND ( 'NONE', #18383, .T. ) ;
#16037 = DIRECTION ( 'NONE',  ( 0.000000000000000000, 0.000000000000000000, 1.000000000000000000 ) ) ;
#16038 = CARTESIAN_POINT ( 'NONE',  ( 124.5381772159375942, -111.0842361345572158, -35.99999999999997158 ) ) ;
#16039 = ORIENTED_EDGE ( 'NONE', *, *, #5511, .T. ) ;
#16040 = DIRECTION ( 'NONE',  ( 0.000000000000000000, 1.000000000000000000, 0.000000000000000000 ) ) ;
#16041 = DIRECTION ( 'NONE',  ( 1.000000000000000000, 0.000000000000000000, 0.000000000000000000 ) ) ;
#16042 = CARTESIAN_POINT ( 'NONE',  ( -48.65098454476478196, 77.46608744949921288, -15.00000000000001421 ) ) ;
#16043 = ORIENTED_EDGE ( 'NONE', *, *, #12022, .F. ) ;
#16044 = CARTESIAN_POINT ( 'NONE',  ( -94.45685920050698314, -2.213358015103445098, 15.00000000000006928 ) ) ;
#16045 = DIRECTION ( 'NONE',  ( 0.9396926207859084279, 0.3420201433256686574, -1.086737899652989892E-16 ) ) ;
#16046 = EDGE_LOOP ( 'NONE', ( #15161, #4663, #17344, #17154 ) ) ;
#16047 = ORIENTED_EDGE ( 'NONE', *, *, #3219, .T. ) ;
#16048 = VERTEX_POINT ( 'NONE', #16331 ) ;
#16049 = PLANE ( 'NONE',  #9975 ) ;
#16050 = CARTESIAN_POINT ( 'NONE',  ( 0.000000000000000000, 0.000000000000000000, 0.000000000000000000 ) ) ;
#16051 = CARTESIAN_POINT ( 'NONE',  ( -52.04298920050707977, 93.78931001713317528, -167.1454815528550739 ) ) ;
#16052 = DIRECTION ( 'NONE',  ( -0.9396926207859097602, 0.3420201433256649937, 0.000000000000000000 ) ) ;
#16053 = CARTESIAN_POINT ( 'NONE',  ( -68.99615306438103346, 32.81108233166271759, -167.1454815528550739 ) ) ;
#16054 = LINE ( 'NONE', #4927, #15949 ) ;
#16055 = EDGE_LOOP ( 'NONE', ( #15754, #5663, #3391 ) ) ;
#16056 = CARTESIAN_POINT ( 'NONE',  ( -57.08002265617300708, 84.22855780814606419, 25.00000000000000355 ) ) ;
#16057 = LINE ( 'NONE', #3336, #15722 ) ;
#16058 = LINE ( 'NONE', #4731, #9730 ) ;
#16059 = DIRECTION ( 'NONE',  ( 1.000000000000000000, 0.000000000000000000, 0.000000000000000000 ) ) ;
#16060 = CARTESIAN_POINT ( 'NONE',  ( -36.10481200028119275, 85.94077383471113762, 55.19394003363846224 ) ) ;
#16061 = DIRECTION ( 'NONE',  ( 0.000000000000000000, 0.000000000000000000, -1.000000000000000000 ) ) ;
#16062 = VERTEX_POINT ( 'NONE', #2303 ) ;
#16063 = DIRECTION ( 'NONE',  ( -1.000000000000000000, 0.000000000000000000, 0.000000000000000000 ) ) ;
#16064 = CARTESIAN_POINT ( 'NONE',  ( -53.29103256796045684, 73.45256821284057480, -15.00000000000001421 ) ) ;
#16065 = ORIENTED_EDGE ( 'NONE', *, *, #4139, .F. ) ;
#16066 = EDGE_CURVE ( 'NONE', #9970, #5754, #13544, .T. ) ;
#16067 = EDGE_LOOP ( 'NONE', ( #1537, #6688, #3980, #16582 ) ) ;
#16068 = AXIS2_PLACEMENT_3D ( 'NONE', #4501, #1524, #7234 ) ;
#16069 = VERTEX_POINT ( 'NONE', #4827 ) ;
#16070 = CARTESIAN_POINT ( 'NONE',  ( -57.08002265617300708, 84.22855780814606419, -15.00000000000001421 ) ) ;
#16071 = DIRECTION ( 'NONE',  ( 1.000000000000000000, 0.000000000000000000, 3.771137991253923150E-16 ) ) ;
#16072 = CARTESIAN_POINT ( 'NONE',  ( -78.10200868170512933, 83.24379415027480889, 55.06081777697277602 ) ) ;
#16073 = DIRECTION ( 'NONE',  ( -1.000000000000000000, -3.016910393003138520E-15, 0.000000000000000000 ) ) ;
#16074 = FACE_OUTER_BOUND ( 'NONE', #18152, .T. ) ;
#16075 = CARTESIAN_POINT ( 'NONE',  ( -71.24615306438104767, 38.27533460456375991, -15.00000000000001421 ) ) ;
#16076 = CARTESIAN_POINT ( 'NONE',  ( -71.24615306438103346, 40.52805651522925245, -167.1454815528550739 ) ) ;
#16077 = VERTEX_POINT ( 'NONE', #731 ) ;
#16078 = CARTESIAN_POINT ( 'NONE',  ( -68.99615306438082030, 80.54982793813024955, 15.00000000000006928 ) ) ;
#16079 = CARTESIAN_POINT ( 'NONE',  ( -71.24615306438082030, 85.39922435456374217, 15.00000000000006928 ) ) ;
#16080 = CARTESIAN_POINT ( 'NONE',  ( -59.22941447913701296, 106.4346967249104239, 102.5000000000000000 ) ) ;
#16081 = VECTOR ( 'NONE', #11811, 1000.000000000000000 ) ;
#16082 = VERTEX_POINT ( 'NONE', #6506 ) ;
#16083 = CARTESIAN_POINT ( 'NONE',  ( -70.27900850916093134, -47.21335801510345220, -15.00000000000001599 ) ) ;
#16084 = CARTESIAN_POINT ( 'NONE',  ( -68.43628269749412141, 57.12909386699050884, 22.41747227276118792 ) ) ;
#16085 = VERTEX_POINT ( 'NONE', #10930 ) ;
#16086 = ORIENTED_EDGE ( 'NONE', *, *, #2084, .F. ) ;
#16087 = CARTESIAN_POINT ( 'NONE',  ( -68.99615306438072082, 139.6252324316626812, -167.1454815528550739 ) ) ;
#16088 = CIRCLE ( 'NONE', #8944, 29.36884788726140627 ) ;
#16089 = DIRECTION ( 'NONE',  ( 0.000000000000000000, 1.000000000000000000, 0.000000000000000000 ) ) ;
#16090 = DIRECTION ( 'NONE',  ( 0.000000000000000000, 0.000000000000000000, 1.000000000000000000 ) ) ;
#16091 = ORIENTED_EDGE ( 'NONE', *, *, #3459, .T. ) ;
#16092 = EDGE_CURVE ( 'NONE', #3553, #7250, #11945, .T. ) ;
#16093 = AXIS2_PLACEMENT_3D ( 'NONE', #804, #16504, #13708 ) ;
#16094 = ORIENTED_EDGE ( 'NONE', *, *, #17886, .F. ) ;
#16095 = CARTESIAN_POINT ( 'NONE',  ( 0.000000000000000000, -5.629165124598996428, -3.250000000000020428 ) ) ;
#16096 = CARTESIAN_POINT ( 'NONE',  ( -66.00585202009864361, 110.8305070361169840, 25.00000000000000355 ) ) ;
#16097 = DIRECTION ( 'NONE',  ( 0.000000000000000000, 0.000000000000000000, -1.000000000000000000 ) ) ;
#16098 = DIRECTION ( 'NONE',  ( -0.000000000000000000, -0.000000000000000000, -1.000000000000000000 ) ) ;
#16099 = VERTEX_POINT ( 'NONE', #10548 ) ;
#16100 = DIRECTION ( 'NONE',  ( 1.000000000000000000, -0.000000000000000000, -0.000000000000000000 ) ) ;
#16101 = ORIENTED_EDGE ( 'NONE', *, *, #5020, .F. ) ;
#16102 = EDGE_CURVE ( 'NONE', #12783, #9284, #10724, .T. ) ;
#16103 = LINE ( 'NONE', #9019, #3234 ) ;
#16104 = ORIENTED_EDGE ( 'NONE', *, *, #459, .T. ) ;
#16106 = EDGE_CURVE ( 'NONE', #10354, #1317, #3432, .T. ) ;
#16105 = AXIS2_PLACEMENT_3D ( 'NONE', #3136, #8848, #7419 ) ;
#16107 = ADVANCED_FACE ( 'NONE', ( #13819 ), #9510, .T. ) ;
#16108 = AXIS2_PLACEMENT_3D ( 'NONE', #16745, #3845, #12278 ) ;
#16109 = ORIENTED_EDGE ( 'NONE', *, *, #4784, .T. ) ;
#16110 = SURFACE_STYLE_USAGE ( .BOTH. , #3395 ) ;
#16111 = DIRECTION ( 'NONE',  ( 0.3822456275483139820, 0.9240607556974786974, 0.000000000000000000 ) ) ;
#16112 = CARTESIAN_POINT ( 'NONE',  ( -68.99615306438109030, 17.10311908166270811, -15.00000000000001421 ) ) ;
#16113 = EDGE_CURVE ( 'NONE', #12461, #10547, #3586, .T. ) ;
#16114 = ORIENTED_EDGE ( 'NONE', *, *, #13172, .T. ) ;
#16115 = EDGE_CURVE ( 'NONE', #16406, #14163, #13168, .T. ) ;
#16116 = EDGE_CURVE ( 'NONE', #10339, #15944, #9604, .T. ) ;
#16117 = CARTESIAN_POINT ( 'NONE',  ( -107.5676225674731938, 110.5691553257988460, 22.35917033480641081 ) ) ;
#16118 = LINE ( 'NONE', #15774, #16460 ) ;
#16119 = AXIS2_PLACEMENT_3D ( 'NONE', #8728, #209, #8634 ) ;
#16120 = CARTESIAN_POINT ( 'NONE',  ( -68.99615306438101925, 33.42593818813028861, -15.00000000000001421 ) ) ;
#16121 = ORIENTED_EDGE ( 'NONE', *, *, #4410, .T. ) ;
#16122 = CARTESIAN_POINT ( 'NONE',  ( -50.41499038512538533, 117.9449492212793444, 2.999999999999999112 ) ) ;
#16123 = VECTOR ( 'NONE', #12830, 1000.000000000000114 ) ;
#16124 = LINE ( 'NONE', #4907, #15893 ) ;
#16125 = CARTESIAN_POINT ( 'NONE',  ( -92.59262256747318531, 50.58224449241411236, -25.00000000000000000 ) ) ;
#16126 = VERTEX_POINT ( 'NONE', #4097 ) ;
#16127 = LINE ( 'NONE', #17351, #6717 ) ;
#16128 = CARTESIAN_POINT ( 'NONE',  ( -75.72335493167710752, 61.53592931583062864, -28.00000000000000355 ) ) ;
#16129 = ORIENTED_EDGE ( 'NONE', *, *, #16155, .T. ) ;
#16130 = EDGE_CURVE ( 'NONE', #11213, #8044, #1110, .T. ) ;
#16131 = VECTOR ( 'NONE', #12153, 1000.000000000000000 ) ;
#16132 = EDGE_CURVE ( 'NONE', #9281, #13601, #18128, .T. ) ;
#16133 = VERTEX_POINT ( 'NONE', #11398 ) ;
#16134 = AXIS2_PLACEMENT_3D ( 'NONE', #15799, #14395, #5874 ) ;
#16135 = AXIS2_PLACEMENT_3D ( 'NONE', #75, #7182, #1206 ) ;
#16136 = ORIENTED_EDGE ( 'NONE', *, *, #15690, .F. ) ;
#16137 = CARTESIAN_POINT ( 'NONE',  ( -66.02736529514692165, 75.49957964911740760, -15.00000000000001243 ) ) ;
#16138 = DIRECTION ( 'NONE',  ( 0.000000000000000000, 1.000000000000000000, 0.000000000000000000 ) ) ;
#16139 =( NAMED_UNIT ( * ) SI_UNIT ( $, .STERADIAN. ) SOLID_ANGLE_UNIT ( ) );
#16140 = CARTESIAN_POINT ( 'NONE',  ( -68.99615306438077766, 117.6340838816626899, -167.1454815528550739 ) ) ;
#16141 = CARTESIAN_POINT ( 'NONE',  ( -63.37199650155329778, 75.44273092821040905, -167.1454815528550739 ) ) ;
#16142 = ORIENTED_EDGE ( 'NONE', *, *, #6030, .F. ) ;
#16143 = VECTOR ( 'NONE', #13225, 1000.000000000000000 ) ;
#16144 = FACE_OUTER_BOUND ( 'NONE', #7897, .T. ) ;
#16145 = FACE_OUTER_BOUND ( 'NONE', #6122, .T. ) ;
#16146 = DIRECTION ( 'NONE',  ( 1.000000000000000000, -0.000000000000000000, -0.000000000000000000 ) ) ;
#16147 = CARTESIAN_POINT ( 'NONE',  ( -55.20348911625212907, 74.15281352429526862, -167.1454815528550739 ) ) ;
#16148 = CARTESIAN_POINT ( 'NONE',  ( -36.62604544348833713, 89.18779308299876618, 56.85266771181889567 ) ) ;
#16149 = ORIENTED_EDGE ( 'NONE', *, *, #17013, .T. ) ;
#16150 = CIRCLE ( 'NONE', #10785, 4.599999999999992539 ) ;
#16151 = VECTOR ( 'NONE', #2096, 1000.000000000000000 ) ;
#16152 = EDGE_CURVE ( 'NONE', #6934, #14227, #1197, .T. ) ;
#16153 = CARTESIAN_POINT ( 'NONE',  ( -67.59262256747319952, 110.5691553257988460, -26.35917033480641436 ) ) ;
#16154 = VERTEX_POINT ( 'NONE', #3996 ) ;
#16155 = EDGE_CURVE ( 'NONE', #15948, #7142, #8502, .T. ) ;
#16156 = PLANE ( 'NONE',  #17621 ) ;
#16157 = ORIENTED_EDGE ( 'NONE', *, *, #7406, .F. ) ;
#16158 = VERTEX_POINT ( 'NONE', #18221 ) ;
#16159 = EDGE_LOOP ( 'NONE', ( #7541, #17750, #14778, #12866 ) ) ;
#16160 = CIRCLE ( 'NONE', #8109, 12.50000000000001776 ) ;
#16161 = CIRCLE ( 'NONE', #12918, 7.168074330098860969 ) ;
#16162 = CARTESIAN_POINT ( 'NONE',  ( -57.08002265617300708, 84.22855780814606419, 15.00000000000006928 ) ) ;
#16163 = CARTESIAN_POINT ( 'NONE',  ( -68.99615306438097662, 61.08541618166268705, -15.00000000000001421 ) ) ;
#16164 = CARTESIAN_POINT ( 'NONE',  ( -70.64221740337633548, 110.2804215074198737, 22.36668740498762276 ) ) ;
#16165 = DIRECTION ( 'NONE',  ( 0.000000000000000000, 1.000000000000000000, 0.000000000000000000 ) ) ;
#16166 = DIRECTION ( 'NONE',  ( -1.000000000000000000, 0.000000000000000000, 0.000000000000000000 ) ) ;
#16167 = CARTESIAN_POINT ( 'NONE',  ( -61.60537251683745552, 75.03273214436880778, 15.00000000000006928 ) ) ;
#16168 = ORIENTED_EDGE ( 'NONE', *, *, #14642, .T. ) ;
#16169 = EDGE_CURVE ( 'NONE', #8923, #18088, #2792, .T. ) ;
#16170 = CARTESIAN_POINT ( 'NONE',  ( -57.08002265617300708, 84.22855780814606419, -167.1454815528550739 ) ) ;
#16171 = CIRCLE ( 'NONE', #14407, 4.600000000000006750 ) ;
#16172 = DIRECTION ( 'NONE',  ( 0.9396926207859171987, 0.3420201433256445100, 4.890320548438495251E-16 ) ) ;
#16173 = CARTESIAN_POINT ( 'NONE',  ( -68.99615306438106188, 26.52789703166272162, -15.00000000000001421 ) ) ;
#16174 = ORIENTED_EDGE ( 'NONE', *, *, #6060, .T. ) ;
#16175 = EDGE_CURVE ( 'NONE', #13941, #5735, #14209, .T. ) ;
#16176 = VECTOR ( 'NONE', #13156, 1000.000000000000000 ) ;
#16177 = CARTESIAN_POINT ( 'NONE',  ( 15.23320273812466574, -111.0842361345572158, 57.00000000000000000 ) ) ;
#16178 = VECTOR ( 'NONE', #13182, 1000.000000000000000 ) ;
#16179 = FACE_OUTER_BOUND ( 'NONE', #2673, .T. ) ;
#16180 = ORIENTED_EDGE ( 'NONE', *, *, #3312, .F. ) ;
#16181 = ORIENTED_EDGE ( 'NONE', *, *, #12489, .T. ) ;
#16182 = AXIS2_PLACEMENT_3D ( 'NONE', #10323, #1534, #17237 ) ;
#16183 = CARTESIAN_POINT ( 'NONE',  ( -46.10942163047475617, 78.23723799236688592, 15.00000000000006928 ) ) ;
#16184 = CARTESIAN_POINT ( 'NONE',  ( -68.99615306438089135, 86.21815738166266385, 15.00000000000006928 ) ) ;
#16185 = CARTESIAN_POINT ( 'NONE',  ( -92.59262256747319952, 50.58224449241410525, -15.00000000000000178 ) ) ;
#16186 = ORIENTED_EDGE ( 'NONE', *, *, #11249, .T. ) ;
#16187 = AXIS2_PLACEMENT_3D ( 'NONE', #2104, #15107, #710 ) ;
#16188 = VECTOR ( 'NONE', #4516, 1000.000000000000114 ) ;
#16189 = DIRECTION ( 'NONE',  ( -0.9396926207859084279, 0.3420201433256686574, 0.000000000000000000 ) ) ;
#16190 = ORIENTED_EDGE ( 'NONE', *, *, #8108, .F. ) ;
#16191 = CARTESIAN_POINT ( 'NONE',  ( -71.24615306438114715, 16.28418605456380419, 15.00000000000006928 ) ) ;
#16192 = DIRECTION ( 'NONE',  ( -1.000000000000000000, 0.000000000000000000, -1.047634945911799121E-14 ) ) ;
#16193 = CARTESIAN_POINT ( 'NONE',  ( -77.13785763070544022, 90.59536451873515261, 58.52851757989075310 ) ) ;
#16194 = CARTESIAN_POINT ( 'NONE',  ( 0.5805565836007609004, -3.752776749732712691, -6.500000000000033751 ) ) ;
#16195 = VERTEX_POINT ( 'NONE', #5582 ) ;
#16196 = PLANE ( 'NONE',  #6857 ) ;
#16197 = ORIENTED_EDGE ( 'NONE', *, *, #4933, .F. ) ;
#16198 = AXIS2_PLACEMENT_3D ( 'NONE', #7687, #13489, #6460 ) ;
#16199 = ADVANCED_FACE ( 'NONE', ( #11216 ), #16905, .F. ) ;
#16200 = CARTESIAN_POINT ( 'NONE',  ( -71.24615306438067819, 144.2006139652292518, -167.1454815528550739 ) ) ;
#16201 = ORIENTED_EDGE ( 'NONE', *, *, #5725, .F. ) ;
#16202 = ADVANCED_FACE ( 'NONE', ( #5302 ), #11089, .F. ) ;
#16203 = AXIS2_PLACEMENT_3D ( 'NONE', #12067, #9348, #9078 ) ;
#16204 = EDGE_LOOP ( 'NONE', ( #17537, #13568, #13930, #1836 ) ) ;
#16205 = AXIS2_PLACEMENT_3D ( 'NONE', #13947, #1131, #5237 ) ;
#16206 = AXIS2_PLACEMENT_3D ( 'NONE', #8263, #18267, #5441 ) ;
#16207 = VERTEX_POINT ( 'NONE', #1009 ) ;
#16208 = CARTESIAN_POINT ( 'NONE',  ( -92.59262256747321373, 110.5691553257988460, -30.35917033480641081 ) ) ;
#16209 = CIRCLE ( 'NONE', #8168, 12.49999999999999112 ) ;
#16210 = ORIENTED_EDGE ( 'NONE', *, *, #10756, .T. ) ;
#16211 = CARTESIAN_POINT ( 'NONE',  ( 45.30000000000000426, 0.000000000000000000, 0.000000000000000000 ) ) ;
#16212 = EDGE_CURVE ( 'NONE', #7430, #12040, #15417, .T. ) ;
#16213 = FACE_OUTER_BOUND ( 'NONE', #16873, .T. ) ;
#16214 = ORIENTED_EDGE ( 'NONE', *, *, #11243, .F. ) ;
#16215 = ADVANCED_FACE ( 'NONE', ( #17091 ), #12802, .T. ) ;
#16216 = CARTESIAN_POINT ( 'NONE',  ( -70.85175816390371040, -141.5628872026273086, 57.00000000000000000 ) ) ;
#16217 = AXIS2_PLACEMENT_3D ( 'NONE', #5781, #6037, #8961 ) ;
#16218 = VECTOR ( 'NONE', #1814, 1000.000000000000000 ) ;
#16219 = ORIENTED_EDGE ( 'NONE', *, *, #15782, .F. ) ;
#16220 = AXIS2_PLACEMENT_3D ( 'NONE', #13809, #12515, #14101 ) ;
#16221 = DIRECTION ( 'NONE',  ( 0.000000000000000000, 1.000000000000000000, 0.000000000000000000 ) ) ;
#16222 = DIRECTION ( 'NONE',  ( 0.000000000000000000, 1.000000000000000000, 0.000000000000000000 ) ) ;
#16223 = DIRECTION ( 'NONE',  ( 1.000000000000000000, 0.000000000000000000, 5.551115123125777772E-16 ) ) ;
#16224 = EDGE_CURVE ( 'NONE', #15944, #16663, #9896, .T. ) ;
#16225 = EDGE_CURVE ( 'NONE', #12749, #10207, #7001, .T. ) ;
#16226 = DIRECTION ( 'NONE',  ( 1.000000000000000000, 0.000000000000000000, 0.000000000000000000 ) ) ;
#16227 = EDGE_CURVE ( 'NONE', #17012, #15460, #18418, .T. ) ;
#16228 = ORIENTED_EDGE ( 'NONE', *, *, #16823, .T. ) ;
#16229 = EDGE_LOOP ( 'NONE', ( #370, #16549, #11195, #8053 ) ) ;
#16230 = AXIS2_PLACEMENT_3D ( 'NONE', #18517, #5687, #11416 ) ;
#16231 = AXIS2_PLACEMENT_3D ( 'NONE', #3509, #9224, #2112 ) ;
#16232 = PRODUCT_DEFINITION_SHAPE ( 'NONE', 'NONE',  #18521 ) ;
#16233 = VERTEX_POINT ( 'NONE', #11651 ) ;
#16234 = CARTESIAN_POINT ( 'NONE',  ( -78.12361985383350316, 84.22855780814607840, 70.00000000000001421 ) ) ;
#16235 = CARTESIAN_POINT ( 'NONE',  ( -71.24615306438091977, 79.11603905456372843, -167.1454815528550739 ) ) ;
#16236 = EDGE_CURVE ( 'NONE', #12009, #16154, #1824, .T. ) ;
#16237 = ORIENTED_EDGE ( 'NONE', *, *, #10177, .F. ) ;
#16238 = SHAPE_DEFINITION_REPRESENTATION ( #8355, #1677 ) ;
#16239 = DIRECTION ( 'NONE',  ( 0.000000000000000000, 0.000000000000000000, 1.000000000000000000 ) ) ;
#16240 = CARTESIAN_POINT ( 'NONE',  ( -50.24148097183213935, 76.59466308582166505, -15.00000000000001421 ) ) ;
#16241 = DIRECTION ( 'NONE',  ( 0.000000000000000000, 0.000000000000000000, 1.000000000000000000 ) ) ;
#16242 = ORIENTED_EDGE ( 'NONE', *, *, #7665, .T. ) ;
#16243 = CARTESIAN_POINT ( 'NONE',  ( -48.21445538031289857, 89.37090336996882911, -167.1454815528550739 ) ) ;
#16244 = CYLINDRICAL_SURFACE ( 'NONE', #16894, 29.36884788726140627 ) ;
#16245 = EDGE_CURVE ( 'NONE', #315, #14448, #13079, .T. ) ;
#16246 = DIRECTION ( 'NONE',  ( 0.000000000000000000, 0.000000000000000000, -1.000000000000000000 ) ) ;
#16247 = FACE_OUTER_BOUND ( 'NONE', #2463, .T. ) ;
#16248 = EDGE_CURVE ( 'NONE', #10547, #9500, #14374, .T. ) ;
#16249 = CARTESIAN_POINT ( 'NONE',  ( -71.24615306438076345, 125.3510580652292248, 15.00000000000006928 ) ) ;
#16250 = VERTEX_POINT ( 'NONE', #4282 ) ;
#16251 = VECTOR ( 'NONE', #11875, 1000.000000000000000 ) ;
#16252 = VECTOR ( 'NONE', #12723, 1000.000000000000000 ) ;
#16253 = CIRCLE ( 'NONE', #9110, 81.86696747278378439 ) ;
#16254 = VECTOR ( 'NONE', #16851, 1000.000000000000114 ) ;
#16255 = DIRECTION ( 'NONE',  ( 0.000000000000000000, 0.000000000000000000, 1.000000000000000000 ) ) ;
#16256 = LINE ( 'NONE', #17756, #12269 ) ;
#16257 = ORIENTED_EDGE ( 'NONE', *, *, #17940, .F. ) ;
#16258 = EDGE_CURVE ( 'NONE', #14160, #17041, #1529, .T. ) ;
#16259 = CARTESIAN_POINT ( 'NONE',  ( -68.99615306438070661, 111.9657544381302046, 15.00000000000006928 ) ) ;
#16260 = CARTESIAN_POINT ( 'NONE',  ( -7.840676406241780860, 112.6569076202650308, 102.5000000000000000 ) ) ;
#16261 = ORIENTED_EDGE ( 'NONE', *, *, #1720, .T. ) ;
#16262 = VERTEX_POINT ( 'NONE', #14556 ) ;
#16263 = VECTOR ( 'NONE', #5177, 1000.000000000000000 ) ;
#16264 = DIRECTION ( 'NONE',  ( 0.000000000000000000, 0.000000000000000000, 1.000000000000000000 ) ) ;
#16265 = AXIS2_PLACEMENT_3D ( 'NONE', #14379, #17193, #4377 ) ;
#16266 = EDGE_LOOP ( 'NONE', ( #10553, #5171, #3013, #2092, #1095, #16237, #7702, #11032 ) ) ;
#16267 = AXIS2_PLACEMENT_3D ( 'NONE', #6071, #13201, #12071 ) ;
#16268 = CIRCLE ( 'NONE', #4899, 10.24900000000000055 ) ;
#16269 = FACE_OUTER_BOUND ( 'NONE', #5763, .T. ) ;
#16270 = CARTESIAN_POINT ( 'NONE',  ( -71.24615306438111872, 19.42577870456376132, -167.1454815528550739 ) ) ;
#16271 = CARTESIAN_POINT ( 'NONE',  ( -70.06856178257680767, 110.5691553257988460, 22.35917033480641791 ) ) ;
#16272 = DIRECTION ( 'NONE',  ( 0.000000000000000000, 0.000000000000000000, 1.000000000000000000 ) ) ;
#16273 = CARTESIAN_POINT ( 'NONE',  ( -51.81614838398844824, 95.01461175692088545, 15.00000000000007105 ) ) ;
#16274 = CARTESIAN_POINT ( 'NONE',  ( -57.08002265617301418, 106.1506877598988154, 102.5000000000000000 ) ) ;
#16275 = ORIENTED_EDGE ( 'NONE', *, *, #6599, .F. ) ;
#16276 = DIRECTION ( 'NONE',  ( 0.000000000000000000, 0.000000000000000000, 1.000000000000000000 ) ) ;
#16277 = DIRECTION ( 'NONE',  ( 0.9396926207859097602, 0.3420201433256649937, -1.086737899652991371E-16 ) ) ;
#16278 = ORIENTED_EDGE ( 'NONE', *, *, #12155, .T. ) ;
#16279 = CARTESIAN_POINT ( 'NONE',  ( -71.24615306438091977, 75.08557566522922855, -167.1454815528550739 ) ) ;
#16280 = CIRCLE ( 'NONE', #8227, 12.49999999999999112 ) ;
#16281 = DIRECTION ( 'NONE',  ( 0.000000000000000000, -5.551115123125747573E-17, -1.000000000000000000 ) ) ;
#16283 = EDGE_LOOP ( 'NONE', ( #12601, #2294, #14819, #12244 ) ) ;
#16282 = AXIS2_PLACEMENT_3D ( 'NONE', #6313, #4924, #7725 ) ;
#16284 = ORIENTED_EDGE ( 'NONE', *, *, #5925, .T. ) ;
#16285 = DIRECTION ( 'NONE',  ( 0.000000000000000000, 0.000000000000000000, 1.000000000000000000 ) ) ;
#16286 = DIRECTION ( 'NONE',  ( 0.9396926207859097602, 0.3420201433256649937, 0.000000000000000000 ) ) ;
#16287 = DIRECTION ( 'NONE',  ( 1.000000000000000000, 0.000000000000000000, 0.000000000000000000 ) ) ;
#16288 = CARTESIAN_POINT ( 'NONE',  ( -57.08002265617300708, 84.22855780814606419, 15.00000000000006928 ) ) ;
#16289 = VERTEX_POINT ( 'NONE', #7267 ) ;
#16290 = LINE ( 'NONE', #17085, #11058 ) ;
#16291 = VECTOR ( 'NONE', #10555, 1000.000000000000114 ) ;
#16292 = AXIS2_PLACEMENT_3D ( 'NONE', #18441, #17015, #7198 ) ;
#16293 = CARTESIAN_POINT ( 'NONE',  ( -107.5926225674731853, 50.58224449241411236, 35.00000000000000000 ) ) ;
#16294 = ORIENTED_EDGE ( 'NONE', *, *, #18288, .T. ) ;
#16295 = CARTESIAN_POINT ( 'NONE',  ( -7.405446926806058452E-14, -96.08423613455721579, 10.65431531532616560 ) ) ;
#16296 = LINE ( 'NONE', #3288, #3615 ) ;
#16297 = CARTESIAN_POINT ( 'NONE',  ( -48.99724571598702738, 77.92691374209489652, -15.00000000000001421 ) ) ;
#16298 = CYLINDRICAL_SURFACE ( 'NONE', #8755, 5.000000000000000000 ) ;
#16299 = EDGE_LOOP ( 'NONE', ( #6332, #4802, #17826, #2005 ) ) ;
#16300 = CARTESIAN_POINT ( 'NONE',  ( -70.27900850916093134, -47.21335801510345220, -15.00000000000001599 ) ) ;
#16301 = EDGE_LOOP ( 'NONE', ( #10184, #17266, #8213, #198 ) ) ;
#16302 = CARTESIAN_POINT ( 'NONE',  ( -71.24615306438094819, 69.69126110456375045, -15.00000000000001421 ) ) ;
#16303 = ORIENTED_EDGE ( 'NONE', *, *, #8719, .F. ) ;
#16304 = EDGE_LOOP ( 'NONE', ( #11268, #12720, #17519, #17321 ) ) ;
#16305 = DIRECTION ( 'NONE',  ( 0.000000000000000000, 0.000000000000000000, -1.000000000000000000 ) ) ;
#16306 = DIRECTION ( 'NONE',  ( 1.000000000000000000, 2.062304371594500494E-16, -2.775557561562890858E-16 ) ) ;
#16307 = ORIENTED_EDGE ( 'NONE', *, *, #11873, .T. ) ;
#16308 = CYLINDRICAL_SURFACE ( 'NONE', #13185, 3.999999999999996447 ) ;
#16309 = DIRECTION ( 'NONE',  ( 0.000000000000000000, 0.000000000000000000, -1.000000000000000000 ) ) ;
#16310 = ORIENTED_EDGE ( 'NONE', *, *, #10593, .T. ) ;
#16311 = ADVANCED_FACE ( 'NONE', ( #6114 ), #3229, .T. ) ;
#16312 = LINE ( 'NONE', #13336, #5706 ) ;
#16313 = ORIENTED_EDGE ( 'NONE', *, *, #2911, .T. ) ;
#16314 = LINE ( 'NONE', #4992, #5731 ) ;
#16315 = CARTESIAN_POINT ( 'NONE',  ( -66.92854697799583619, 108.0100032524460261, 25.00000000000000355 ) ) ;
#16316 = ORIENTED_EDGE ( 'NONE', *, *, #13340, .F. ) ;
#16317 = DIRECTION ( 'NONE',  ( 0.000000000000000000, 1.000000000000000000, 0.000000000000000000 ) ) ;
#16318 = LINE ( 'NONE', #13805, #10145 ) ;
#16319 = VERTEX_POINT ( 'NONE', #11576 ) ;
#16320 = ADVANCED_FACE ( 'NONE', ( #14292 ), #1734, .T. ) ;
#16321 = ORIENTED_EDGE ( 'NONE', *, *, #10197, .T. ) ;
#16322 = DIRECTION ( 'NONE',  ( 1.000000000000000000, 0.000000000000000000, 0.000000000000000000 ) ) ;
#16323 = LINE ( 'NONE', #10922, #17424 ) ;
#16324 = ORIENTED_EDGE ( 'NONE', *, *, #9164, .T. ) ;
#16325 = CARTESIAN_POINT ( 'NONE',  ( -71.24615306438070661, 147.3422066152292871, -167.1454815528550739 ) ) ;
#16326 = CARTESIAN_POINT ( 'NONE',  ( -71.24615306438109030, 25.70896400456376796, 15.00000000000006928 ) ) ;
#16327 = DIRECTION ( 'NONE',  ( 0.000000000000000000, 0.000000000000000000, 1.000000000000000000 ) ) ;
#16328 = VERTEX_POINT ( 'NONE', #2886 ) ;
#16329 = EDGE_CURVE ( 'NONE', #1178, #6902, #7437, .T. ) ;
#16330 = ADVANCED_FACE ( 'NONE', ( #13153 ), #1468, .T. ) ;
#16331 = CARTESIAN_POINT ( 'NONE',  ( -68.99615306438100504, 39.09426763166271002, -15.00000000000001421 ) ) ;
#16332 = CARTESIAN_POINT ( 'NONE',  ( -68.99615306438100504, 42.23586028166270978, 15.00000000000006928 ) ) ;
#16333 = CARTESIAN_POINT ( 'NONE',  ( -123.4618227840623632, -111.0842361345572158, 36.00000000000001421 ) ) ;
#16334 = CARTESIAN_POINT ( 'NONE',  ( -64.40194603863702127, 76.28065702765842104, 15.00000000000006928 ) ) ;
#16335 = ORIENTED_EDGE ( 'NONE', *, *, #8238, .T. ) ;
#16336 = EDGE_CURVE ( 'NONE', #9679, #4169, #7174, .T. ) ;
#16337 = LINE ( 'NONE', #9335, #3723 ) ;
#16338 = CARTESIAN_POINT ( 'NONE',  ( -64.65314733921417201, -94.06000665574430286, 44.58117175117424580 ) ) ;
#16339 = ORIENTED_EDGE ( 'NONE', *, *, #8089, .T. ) ;
#16340 = LINE ( 'NONE', #3528, #4197 ) ;
#16341 = ADVANCED_FACE ( 'NONE', ( #5860 ), #12895, .T. ) ;
#16342 = DIRECTION ( 'NONE',  ( -1.000000000000000000, -1.895687670108323806E-14, 1.692578276882432005E-16 ) ) ;
#16343 = EDGE_LOOP ( 'NONE', ( #1722, #2812, #16109, #11256 ) ) ;
#16344 = EDGE_CURVE ( 'NONE', #6741, #15230, #12904, .T. ) ;
#16345 = ORIENTED_EDGE ( 'NONE', *, *, #1307, .F. ) ;
#16346 = EDGE_CURVE ( 'NONE', #1716, #12432, #17186, .T. ) ;
#16347 = ADVANCED_FACE ( 'NONE', ( #15777 ), #14471, .T. ) ;
#16348 = DIRECTION ( 'NONE',  ( -0.9396926207859022107, 0.3420201433256853663, -4.890320548438416365E-16 ) ) ;
#16349 = VERTEX_POINT ( 'NONE', #327 ) ;
#16350 = LINE ( 'NONE', #4847, #11792 ) ;
#16351 = CARTESIAN_POINT ( 'NONE',  ( -69.37109144396066540, 81.95267818613797317, -15.00000000000001421 ) ) ;
#16352 = CARTESIAN_POINT ( 'NONE',  ( -70.35643127740523539, 110.4272069818263446, 22.35917033480641436 ) ) ;
#16353 = EDGE_CURVE ( 'NONE', #8597, #3211, #8768, .T. ) ;
#16354 = EDGE_CURVE ( 'NONE', #1460, #14653, #10348, .T. ) ;
#16355 = DIRECTION ( 'NONE',  ( 1.000000000000000000, -0.000000000000000000, -0.000000000000000000 ) ) ;
#16356 = DIRECTION ( 'NONE',  ( -5.204170427930409450E-16, 0.000000000000000000, 1.000000000000000000 ) ) ;
#16357 = DIRECTION ( 'NONE',  ( 0.000000000000000000, 0.000000000000000000, -1.000000000000000000 ) ) ;
#16358 = VERTEX_POINT ( 'NONE', #16497 ) ;
#16359 = CARTESIAN_POINT ( 'NONE',  ( -75.29929411668209127, 61.19352203925132017, -24.09877121037940739 ) ) ;
#16360 = DIRECTION ( 'NONE',  ( 0.000000000000000000, 0.000000000000000000, -1.000000000000000000 ) ) ;
#16361 = ORIENTED_EDGE ( 'NONE', *, *, #17608, .F. ) ;
#16362 = CYLINDRICAL_SURFACE ( 'NONE', #15990, 7.168074330098860969 ) ;
#16363 = CARTESIAN_POINT ( 'NONE',  ( -68.99615306438106188, 30.28434553813027108, 15.00000000000006928 ) ) ;
#16364 = EDGE_LOOP ( 'NONE', ( #6802, #18197, #14304, #7859 ) ) ;
#16365 = VECTOR ( 'NONE', #16578, 1000.000000000000000 ) ;
#16366 = EDGE_CURVE ( 'NONE', #8650, #8537, #15001, .T. ) ;
#16367 = EDGE_CURVE ( 'NONE', #12161, #9136, #12122, .T. ) ;
#16368 = ORIENTED_EDGE ( 'NONE', *, *, #15457, .F. ) ;
#16369 = DIRECTION ( 'NONE',  ( 1.000000000000000000, 0.000000000000000000, -0.000000000000000000 ) ) ;
#16370 = LINE ( 'NONE', #770, #82 ) ;
#16371 = CARTESIAN_POINT ( 'NONE',  ( -40.55373863553682412, 54.08738549153932951, -24.45531647972368461 ) ) ;
#16372 = CARTESIAN_POINT ( 'NONE',  ( -71.24615306438100504, 53.09442711522921599, 15.00000000000006928 ) ) ;
#16373 = ORIENTED_EDGE ( 'NONE', *, *, #7425, .F. ) ;
#16374 = DIRECTION ( 'NONE',  ( -1.000000000000000000, 0.000000000000000000, 1.692578276882434470E-16 ) ) ;
#16375 = LINE ( 'NONE', #775, #3629 ) ;
#16376 = EDGE_LOOP ( 'NONE', ( #16391, #4846, #9009, #5328 ) ) ;
#16377 = AXIS2_PLACEMENT_3D ( 'NONE', #6543, #946, #6646 ) ;
#16378 = CARTESIAN_POINT ( 'NONE',  ( -107.5926225674731711, 57.88796029049330372, 26.35917033480641436 ) ) ;
#16379 = CARTESIAN_POINT ( 'NONE',  ( -97.59262256747319952, 50.58224449241411236, -25.00000000000000000 ) ) ;
#16380 = CARTESIAN_POINT ( 'NONE',  ( -78.03762390449695374, 86.19059744224304609, 55.24421449531139672 ) ) ;
#16381 = CARTESIAN_POINT ( 'NONE',  ( -68.99615306438094819, 55.41708673813027985, 15.00000000000006928 ) ) ;
#16382 = ORIENTED_EDGE ( 'NONE', *, *, #7655, .F. ) ;
#16383 = DIRECTION ( 'NONE',  ( -5.204170427930409450E-16, 0.000000000000000000, 1.000000000000000000 ) ) ;
#16384 = ORIENTED_EDGE ( 'NONE', *, *, #6881, .F. ) ;
#16385 = CARTESIAN_POINT ( 'NONE',  ( -71.24615306438070661, 147.3422066152292871, 15.00000000000006928 ) ) ;
#16386 = ORIENTED_EDGE ( 'NONE', *, *, #7763, .F. ) ;
#16387 = VECTOR ( 'NONE', #5385, 1000.000000000000000 ) ;
#16388 = ORIENTED_EDGE ( 'NONE', *, *, #14845, .F. ) ;
#16389 = CARTESIAN_POINT ( 'NONE',  ( -68.99615306438094819, 51.66063823166267355, -167.1454815528550739 ) ) ;
#16390 = DIRECTION ( 'NONE',  ( -1.000000000000000000, -0.000000000000000000, -0.000000000000000000 ) ) ;
#16391 = ORIENTED_EDGE ( 'NONE', *, *, #5621, .T. ) ;
#16392 = DIRECTION ( 'NONE',  ( -1.000000000000000000, 0.000000000000000000, 0.000000000000000000 ) ) ;
#16393 = DIRECTION ( 'NONE',  ( -1.000000000000000000, 0.000000000000000000, 0.000000000000000000 ) ) ;
#16394 = ORIENTED_EDGE ( 'NONE', *, *, #10168, .F. ) ;
#16395 = CARTESIAN_POINT ( 'NONE',  ( 0.000000000000000000, -96.08423613455721579, -10.65431531532567710 ) ) ;
#16396 = B_SPLINE_CURVE_WITH_KNOTS ( 'NONE', 3,
 ( #9584, #5565, #6876, #2284, #9783, #883, #13702, #15485, #987, #16600, #7988, #3788, #2372, #8083, #1272, #13800, #13905, #6586, #12309, #18003, #3972, #5190, #10910, #8187, #1096, #12415 ),
 .UNSPECIFIED., .F., .F.,
 ( 4, 2, 2, 2, 2, 2, 2, 2, 2, 2, 2, 2, 4 ),
 ( 0.002699315152504066541, 0.004048330729320218091, 0.005397346306136370508, 0.006746361882952522059, 0.008095377459768675343, 0.008769885248176737674, 0.009444393036584803475, 0.01011890082499286928, 0.01079340861340093508, 0.01146791640180900088, 0.01214242419021706668, 0.01281693197862512901, 0.01349143976703319481 ),
 .UNSPECIFIED. ) ;
#16397 = ORIENTED_EDGE ( 'NONE', *, *, #15575, .F. ) ;
#16398 = VECTOR ( 'NONE', #48, 1000.000000000000000 ) ;
#16399 = CARTESIAN_POINT ( 'NONE',  ( -71.24615306438101925, 28.85055665456376062, 15.00000000000006928 ) ) ;
#16400 = PLANE ( 'NONE',  #17687 ) ;
#16402 = ORIENTED_EDGE ( 'NONE', *, *, #10821, .F. ) ;
#16401 = EDGE_CURVE ( 'NONE', #4700, #2247, #13522, .T. ) ;
#16403 = AXIS2_PLACEMENT_3D ( 'NONE', #13677, #17788, #16374 ) ;
#16404 = DIRECTION ( 'NONE',  ( 0.9396926207859148672, 0.3420201433256507273, -1.086737899652997288E-16 ) ) ;
#16405 = CARTESIAN_POINT ( 'NONE',  ( -107.5926225674731711, 57.88796029049330372, -26.35917033480641436 ) ) ;
#16406 = VERTEX_POINT ( 'NONE', #6296 ) ;
#16407 = ORIENTED_EDGE ( 'NONE', *, *, #9280, .F. ) ;
#16408 = VECTOR ( 'NONE', #657, 1000.000000000000000 ) ;
#16409 = CARTESIAN_POINT ( 'NONE',  ( -68.99615306438099083, 24.00116023813024313, 15.00000000000006928 ) ) ;
#16410 = FACE_OUTER_BOUND ( 'NONE', #4215, .T. ) ;
#16411 = ORIENTED_EDGE ( 'NONE', *, *, #10528, .F. ) ;
#16412 = VECTOR ( 'NONE', #3168, 1000.000000000000000 ) ;
#16413 = CARTESIAN_POINT ( 'NONE',  ( -71.24615306438106188, 35.13374195456378146, -15.00000000000001421 ) ) ;
#16414 = SHAPE_REPRESENTATION_RELATIONSHIP ( 'NONE' , 'NONE' ,  #15553, #6556 ) ;
#16415 = CARTESIAN_POINT ( 'NONE',  ( -77.26467526001188446, 78.27079066365617166, 67.08227311674674809 ) ) ;
#16416 = CARTESIAN_POINT ( 'NONE',  ( 2.646962709418357207, -0.2171425501261921576, 50.59379564821414732 ) ) ;
#16417 = CARTESIAN_POINT ( 'NONE',  ( -68.99615306438072082, 130.2004544816626890, -167.1454815528550739 ) ) ;
#16418 = VERTEX_POINT ( 'NONE', #12023 ) ;
#16419 = CARTESIAN_POINT ( 'NONE',  ( -68.99615306438086293, 89.35975003166268493, -15.00000000000001421 ) ) ;
#16420 = DIRECTION ( 'NONE',  ( 1.000000000000000000, 0.000000000000000000, 0.000000000000000000 ) ) ;
#16421 = FILL_AREA_STYLE ('',( #9430 ) ) ;
#16422 = CARTESIAN_POINT ( 'NONE',  ( -36.44155368744861079, 56.74635804676026396, 22.50216374311547440 ) ) ;
#16423 = ORIENTED_EDGE ( 'NONE', *, *, #13813, .F. ) ;
#16424 = B_SPLINE_CURVE_WITH_KNOTS ( 'NONE', 3,
 ( #966, #6667, #11997, #4974, #3384, #14890, #10781, #1992, #3570, #7970, #3485, #5164, #16476, #9109, #7881, #10688, #10879, #12389, #13684, #10604 ),
 .UNSPECIFIED., .F., .F.,
 ( 4, 2, 2, 2, 2, 2, 2, 2, 2, 4 ),
 ( 0.000000000000000000, 0.001278592738658798026, 0.002557185477317596052, 0.003835778215976394078, 0.005114370954635192104, 0.006392963693293989696, 0.007671556431952788156, 0.008950149170611586616, 0.009589445539940984545, 0.01022874190927038421 ),
 .UNSPECIFIED. ) ;
#16425 = DIRECTION ( 'NONE',  ( 1.558623840612994987E-16, 1.000000000000000000, 0.000000000000000000 ) ) ;
#16426 = DIRECTION ( 'NONE',  ( 0.000000000000000000, 0.000000000000000000, 1.000000000000000000 ) ) ;
#16427 = VECTOR ( 'NONE', #17019, 1000.000000000000000 ) ;
#16428 = EDGE_LOOP ( 'NONE', ( #1544, #5638, #11862, #2662 ) ) ;
#16429 = FACE_BOUND ( 'NONE', #1639, .T. ) ;
#16430 = AXIS2_PLACEMENT_3D ( 'NONE', #13011, #17367, #1672 ) ;
#16431 = VERTEX_POINT ( 'NONE', #17718 ) ;
#16432 = AXIS2_PLACEMENT_3D ( 'NONE', #1861, #4840, #7386 ) ;
#16433 = ORIENTED_EDGE ( 'NONE', *, *, #7547, .F. ) ;
#16434 = ADVANCED_FACE ( 'NONE', ( #4711 ), #3311, .T. ) ;
#16435 = CARTESIAN_POINT ( 'NONE',  ( 276.3098885457529832, -32.62665103886256190, -7.000000000000010658 ) ) ;
#16436 = CIRCLE ( 'NONE', #5689, 47.49926016644912607 ) ;
#16437 = ORIENTED_EDGE ( 'NONE', *, *, #10508, .T. ) ;
#16438 = CARTESIAN_POINT ( 'NONE',  ( -57.08002265617300708, 84.22855780814606419, -35.00000000000000000 ) ) ;
#16439 = CARTESIAN_POINT ( 'NONE',  ( -72.03667955647439669, 58.95149196695728477, 22.49965440599313737 ) ) ;
#16440 = AXIS2_PLACEMENT_3D ( 'NONE', #16622, #13932, #5309 ) ;
#16441 = LINE ( 'NONE', #3632, #1603 ) ;
#16442 = FACE_OUTER_BOUND ( 'NONE', #2336, .T. ) ;
#16444 = EDGE_CURVE ( 'NONE', #18394, #3838, #13481, .T. ) ;
#16443 = VECTOR ( 'NONE', #6393, 1000.000000000000000 ) ;
#16445 = DIRECTION ( 'NONE',  ( -0.000000000000000000, -0.000000000000000000, -1.000000000000000000 ) ) ;
#16446 = CARTESIAN_POINT ( 'NONE',  ( -66.56323152365561668, 80.34130291867722917, 15.00000000000006928 ) ) ;
#16447 = ORIENTED_EDGE ( 'NONE', *, *, #890, .T. ) ;
#16448 = EDGE_CURVE ( 'NONE', #3111, #10621, #2193, .T. ) ;
#16449 = EDGE_CURVE ( 'NONE', #13818, #315, #12609, .T. ) ;
#16450 = FACE_OUTER_BOUND ( 'NONE', #12565, .T. ) ;
#16451 = PLANE ( 'NONE',  #9575 ) ;
#16452 = ORIENTED_EDGE ( 'NONE', *, *, #8266, .T. ) ;
#16453 = AXIS2_PLACEMENT_3D ( 'NONE', #7506, #3287, #11994 ) ;
#16454 = CARTESIAN_POINT ( 'NONE',  ( -26.55110732739451507, -93.39009773859100960, -6.425137615056142337 ) ) ;
#16455 = CARTESIAN_POINT ( 'NONE',  ( -71.24615306438117557, 2.828944715229236628, -167.1454815528550739 ) ) ;
#16456 = ORIENTED_EDGE ( 'NONE', *, *, #8953, .F. ) ;
#16457 = EDGE_CURVE ( 'NONE', #16126, #10978, #16312, .T. ) ;
#16458 = ADVANCED_FACE ( 'NONE', ( #9036 ), #603, .T. ) ;
#16459 = ADVANCED_FACE ( 'NONE', ( #2006 ), #2280, .T. ) ;
#16460 = VECTOR ( 'NONE', #11572, 1000.000000000000114 ) ;
#16461 = ORIENTED_EDGE ( 'NONE', *, *, #1720, .F. ) ;
#16462 = EDGE_CURVE ( 'NONE', #11084, #2797, #17070, .T. ) ;
#16463 = DIRECTION ( 'NONE',  ( 0.000000000000000000, 0.000000000000000000, 1.000000000000000000 ) ) ;
#16464 = LINE ( 'NONE', #7962, #17106 ) ;
#16465 = CARTESIAN_POINT ( 'NONE',  ( -47.49688818721907069, 51.11831089686643281, -26.54642412129686946 ) ) ;
#16466 = DIRECTION ( 'NONE',  ( 0.000000000000000000, 0.000000000000000000, 1.000000000000000000 ) ) ;
#16467 = EDGE_CURVE ( 'NONE', #16250, #800, #17945, .T. ) ;
#16468 = ORIENTED_EDGE ( 'NONE', *, *, #128, .T. ) ;
#16469 = CIRCLE ( 'NONE', #3929, 4.600000000000006750 ) ;
#16470 = CARTESIAN_POINT ( 'NONE',  ( -30.92682688279126424, 73.26749283227019305, 97.49999999999998579 ) ) ;
#16471 = LINE ( 'NONE', #11992, #11102 ) ;
#16472 = ORIENTED_EDGE ( 'NONE', *, *, #10065, .T. ) ;
#16473 = CARTESIAN_POINT ( 'NONE',  ( -68.12361985383350316, 84.22855780814606419, -47.50000000000000000 ) ) ;
#16474 = CARTESIAN_POINT ( 'NONE',  ( -66.40868851600848188, 112.0764521540501875, 25.00000000000000355 ) ) ;
#16475 = CARTESIAN_POINT ( 'NONE',  ( -57.08002265617300708, 84.22855780814606419, -15.00000000000001421 ) ) ;
#16476 = CARTESIAN_POINT ( 'NONE',  ( -112.0226416184558076, -91.42293805878655633, 8.824452519952380669 ) ) ;
#16477 = CIRCLE ( 'NONE', #659, 7.500000000000000000 ) ;
#16478 = VECTOR ( 'NONE', #8258, 1000.000000000000000 ) ;
#16479 = ORIENTED_EDGE ( 'NONE', *, *, #9454, .T. ) ;
#16480 = EDGE_CURVE ( 'NONE', #11833, #10611, #16150, .T. ) ;
#16481 = EDGE_CURVE ( 'NONE', #9020, #12176, #10704, .T. ) ;
#16482 = CARTESIAN_POINT ( 'NONE',  ( -207.6107609645051753, 84.22855780814606419, 50.20642594383511437 ) ) ;
#16483 = ORIENTED_EDGE ( 'NONE', *, *, #4473, .T. ) ;
#16484 = DIRECTION ( 'NONE',  ( 0.000000000000000000, 0.000000000000000000, 1.000000000000000000 ) ) ;
#16485 = VERTEX_POINT ( 'NONE', #16122 ) ;
#16486 = AXIS2_PLACEMENT_3D ( 'NONE', #9898, #16704, #2795 ) ;
#16487 = VERTEX_POINT ( 'NONE', #7905 ) ;
#16488 = AXIS2_PLACEMENT_3D ( 'NONE', #16042, #14558, #14640 ) ;
#16489 = VECTOR ( 'NONE', #14038, 1000.000000000000000 ) ;
#16490 = DIRECTION ( 'NONE',  ( 0.000000000000000000, 1.000000000000000000, 0.000000000000000000 ) ) ;
#16491 = LINE ( 'NONE', #7894, #15631 ) ;
#16492 = ORIENTED_EDGE ( 'NONE', *, *, #5514, .F. ) ;
#16493 = DIRECTION ( 'NONE',  ( 0.000000000000000000, 0.000000000000000000, 1.000000000000000000 ) ) ;
#16494 = FACE_OUTER_BOUND ( 'NONE', #7420, .T. ) ;
#16495 = ORIENTED_EDGE ( 'NONE', *, *, #9742, .T. ) ;
#16496 = AXIS2_PLACEMENT_3D ( 'NONE', #12402, #9773, #1258 ) ;
#16497 = CARTESIAN_POINT ( 'NONE',  ( -71.24615306438070661, 141.0590213152292449, 15.00000000000006928 ) ) ;
#16498 = ORIENTED_EDGE ( 'NONE', *, *, #13285, .T. ) ;
#16499 = DIRECTION ( 'NONE',  ( 0.9396926207859097602, 0.3420201433256649381, 4.890320548438455808E-16 ) ) ;
#16500 = CARTESIAN_POINT ( 'NONE',  ( -68.99615306438077766, 111.9657544381302330, -167.1454815528550739 ) ) ;
#16501 = EDGE_LOOP ( 'NONE', ( #9405, #12517 ) ) ;
#16502 = VECTOR ( 'NONE', #14906, 1000.000000000000000 ) ;
#16503 = LINE ( 'NONE', #6589, #13592 ) ;
#16504 = DIRECTION ( 'NONE',  ( 1.119176436114069332E-16, -1.000000000000000000, -0.000000000000000000 ) ) ;
#16505 = VERTEX_POINT ( 'NONE', #13615 ) ;
#16506 = VECTOR ( 'NONE', #11942, 1000.000000000000000 ) ;
#16507 = ORIENTED_EDGE ( 'NONE', *, *, #4456, .F. ) ;
#16509 = ADVANCED_FACE ( 'NONE', ( #10430 ), #796, .F. ) ;
#16508 = LINE ( 'NONE', #3711, #4307 ) ;
#16510 = CARTESIAN_POINT ( 'NONE',  ( -47.88253357122329845, 84.22855780814606419, 92.50000000000000000 ) ) ;
#16511 = ORIENTED_EDGE ( 'NONE', *, *, #17048, .T. ) ;
#16512 = CIRCLE ( 'NONE', #14711, 4.599999999999992539 ) ;
#16513 = CIRCLE ( 'NONE', #18338, 4.025000000000000355 ) ;
#16514 = ORIENTED_EDGE ( 'NONE', *, *, #13744, .F. ) ;
#16516 = CIRCLE ( 'NONE', #7270, 10.24900000000000766 ) ;
#16515 = CARTESIAN_POINT ( 'NONE',  ( -78.12361985383350316, 84.22855780814606419, 55.00000000000001421 ) ) ;
#16517 = CARTESIAN_POINT ( 'NONE',  ( -0.2223658127159511277, 8.412189173444385659, 47.97586337870632178 ) ) ;
#16518 = CARTESIAN_POINT ( 'NONE',  ( -52.17699016282484337, 93.22868410554724505, 15.00000000000006928 ) ) ;
#16519 = EDGE_LOOP ( 'NONE', ( #8954, #9272, #9767, #6890 ) ) ;
#16520 = FACE_BOUND ( 'NONE', #9293, .T. ) ;
#16521 = DIRECTION ( 'NONE',  ( 1.156482317317869999E-16, 0.000000000000000000, 1.000000000000000000 ) ) ;
#16522 = CARTESIAN_POINT ( 'NONE',  ( -92.59262256747319952, 50.58224449241410525, 35.00000000000000000 ) ) ;
#16523 = CARTESIAN_POINT ( 'NONE',  ( -32.61407059759434190, 55.22775151712274777, 23.63987630418073138 ) ) ;
#16524 = ORIENTED_EDGE ( 'NONE', *, *, #5589, .T. ) ;
#16525 = DIRECTION ( 'NONE',  ( 0.000000000000000000, 0.000000000000000000, 1.000000000000000000 ) ) ;
#16526 = CARTESIAN_POINT ( 'NONE',  ( -68.99615306438086293, 89.35975003166268493, 15.00000000000006928 ) ) ;
#16527 = VERTEX_POINT ( 'NONE', #10801 ) ;
#16528 = AXIS2_PLACEMENT_3D ( 'NONE', #3240, #14486, #5950 ) ;
#16529 = FACE_BOUND ( 'NONE', #3366, .T. ) ;
#16530 = AXIS2_PLACEMENT_3D ( 'NONE', #7085, #1383, #9792 ) ;
#16531 = CARTESIAN_POINT ( 'NONE',  ( -37.41840813535210941, 76.72829797731419887, 62.98988081692781549 ) ) ;
#16532 = ORIENTED_EDGE ( 'NONE', *, *, #15713, .T. ) ;
#16533 = CIRCLE ( 'NONE', #16839, 4.600000000000006750 ) ;
#16534 = EDGE_LOOP ( 'NONE', ( #11008, #14348, #11734, #4946, #5008, #12308, #12110 ) ) ;
#16535 = DIRECTION ( 'NONE',  ( -1.000000000000000000, 0.000000000000000000, 0.000000000000000000 ) ) ;
#16536 = ORIENTED_EDGE ( 'NONE', *, *, #11257, .T. ) ;
#16537 = CARTESIAN_POINT ( 'NONE',  ( -57.08002265617300708, 84.22855780814606419, 15.00000000000006928 ) ) ;
#16538 = CARTESIAN_POINT ( 'NONE',  ( -72.85080879164550538, 59.45131026333987023, 22.67300586969097154 ) ) ;
#16539 = CARTESIAN_POINT ( 'NONE',  ( -67.37428258903915435, 61.13748432492121765, -28.00000000000000000 ) ) ;
#16540 = DIRECTION ( 'NONE',  ( 0.000000000000000000, 0.000000000000000000, 1.000000000000000000 ) ) ;
#16541 = AXIS2_PLACEMENT_3D ( 'NONE', #5300, #900, #15304 ) ;
#16542 = DIRECTION ( 'NONE',  ( 1.000000000000000000, 0.000000000000000000, 0.000000000000000000 ) ) ;
#16543 = AXIS2_PLACEMENT_3D ( 'NONE', #13869, #5432, #7963 ) ;
#16544 = CARTESIAN_POINT ( 'NONE',  ( -71.24615306438103346, 43.66964916522919538, -15.00000000000001421 ) ) ;
#16545 = ORIENTED_EDGE ( 'NONE', *, *, #3676, .F. ) ;
#16546 = EDGE_CURVE ( 'NONE', #12660, #3213, #9408, .T. ) ;
#16547 = DIRECTION ( 'NONE',  ( 3.223492141267075737E-15, 0.000000000000000000, -1.000000000000000000 ) ) ;
#16548 = PLANE ( 'NONE',  #10467 ) ;
#16549 = ORIENTED_EDGE ( 'NONE', *, *, #17503, .F. ) ;
#16550 = CIRCLE ( 'NONE', #13573, 3.999999999999989786 ) ;
#16551 = DIRECTION ( 'NONE',  ( 0.000000000000000000, -1.000000000000000000, 4.000800291689476254E-17 ) ) ;
#16552 = DIRECTION ( 'NONE',  ( 1.000000000000000000, 0.000000000000000000, 5.551115123125784674E-16 ) ) ;
#16553 = EDGE_LOOP ( 'NONE', ( #971, #15444, #15165, #542 ) ) ;
#16554 = ORIENTED_EDGE ( 'NONE', *, *, #14516, .F. ) ;
#16555 = VECTOR ( 'NONE', #11796, 999.9999999999998863 ) ;
#16556 = VECTOR ( 'NONE', #16646, 1000.000000000000000 ) ;
#16557 = ADVANCED_FACE ( 'NONE', ( #1093 ), #12593, .T. ) ;
#16558 = ORIENTED_EDGE ( 'NONE', *, *, #4285, .T. ) ;
#16559 = UNCERTAINTY_MEASURE_WITH_UNIT (LENGTH_MEASURE( 1.000000000000000082E-05 ), #443, 'distance_accuracy_value', 'NONE');
#16560 = FACE_OUTER_BOUND ( 'NONE', #4124, .T. ) ;
#16561 = CARTESIAN_POINT ( 'NONE',  ( -68.99615306438072082, 133.3420471316626958, -167.1454815528550739 ) ) ;
#16562 = DIRECTION ( 'NONE',  ( 0.000000000000000000, 0.000000000000000000, 1.000000000000000000 ) ) ;
#16563 = DIRECTION ( 'NONE',  ( 0.3420201433256686574, 0.9396926207859084279, -0.000000000000000000 ) ) ;
#16564 = CARTESIAN_POINT ( 'NONE',  ( 79.02261728059691848, -151.5628872026273086, -57.00000000000000000 ) ) ;
#16565 = PLANE ( 'NONE',  #354 ) ;
#16566 = ORIENTED_EDGE ( 'NONE', *, *, #8223, .T. ) ;
#16567 = AXIS2_PLACEMENT_3D ( 'NONE', #11582, #7369, #11498 ) ;
#16568 = ADVANCED_FACE ( 'NONE', ( #5185 ), #2668, .T. ) ;
#16569 = DIRECTION ( 'NONE',  ( 0.9396926207859110924, 0.3420201433256611634, 0.000000000000000000 ) ) ;
#16570 = DIRECTION ( 'NONE',  ( 1.000000000000000000, -0.000000000000000000, 5.204170427930409450E-16 ) ) ;
#16572 = VERTEX_POINT ( 'NONE', #2763 ) ;
#16571 = CARTESIAN_POINT ( 'NONE',  ( -68.99615306438110451, 20.85956758813031087, -15.00000000000001421 ) ) ;
#16573 = EDGE_CURVE ( 'NONE', #17232, #6896, #15286, .T. ) ;
#16574 = DIRECTION ( 'NONE',  ( -0.000000000000000000, -0.000000000000000000, -1.000000000000000000 ) ) ;
#16575 = AXIS2_PLACEMENT_3D ( 'NONE', #14494, #9823, #1580 ) ;
#16576 = CARTESIAN_POINT ( 'NONE',  ( -70.71978124295696944, -91.08423613455721579, 5.204170427930421283E-15 ) ) ;
#16577 = ORIENTED_EDGE ( 'NONE', *, *, #17697, .F. ) ;
#16578 = DIRECTION ( 'NONE',  ( 0.000000000000000000, 1.000000000000000000, 0.000000000000000000 ) ) ;
#16579 = EDGE_LOOP ( 'NONE', ( #2620, #13649 ) ) ;
#16580 = ADVANCED_FACE ( 'NONE', ( #1370 ), #6686, .T. ) ;
#16581 = EDGE_CURVE ( 'NONE', #16893, #2633, #1236, .T. ) ;
#16582 = ORIENTED_EDGE ( 'NONE', *, *, #1052, .F. ) ;
#16583 = CIRCLE ( 'NONE', #8553, 12.50000000000000355 ) ;
#16584 = ADVANCED_FACE ( 'NONE', ( #8183 ), #5282, .T. ) ;
#16585 = AXIS2_PLACEMENT_3D ( 'NONE', #11019, #13641, #819 ) ;
#16586 = LINE ( 'NONE', #9477, #9694 ) ;
#16587 = ADVANCED_FACE ( 'NONE', ( #10993 ), #18395, .T. ) ;
#16588 = LINE ( 'NONE', #2659, #5791 ) ;
#16589 = DIRECTION ( 'NONE',  ( 0.3420201433256724322, -0.9396926207859070956, 0.000000000000000000 ) ) ;
#16590 = ORIENTED_EDGE ( 'NONE', *, *, #9619, .T. ) ;
#16591 = DIRECTION ( 'NONE',  ( 0.000000000000000000, 0.000000000000000000, 1.000000000000000000 ) ) ;
#16592 = CARTESIAN_POINT ( 'NONE',  ( -57.08002265617300708, 84.22855780814606419, -15.00000000000001421 ) ) ;
#16593 = CARTESIAN_POINT ( 'NONE',  ( -56.41614838398844256, 95.01461175692088545, -15.00000000000001421 ) ) ;
#16594 = ORIENTED_EDGE ( 'NONE', *, *, #6488, .T. ) ;
#16595 = EDGE_CURVE ( 'NONE', #11655, #17058, #12502, .T. ) ;
#16596 = DIRECTION ( 'NONE',  ( 1.000000000000000000, 0.000000000000000000, 3.771137991253934490E-16 ) ) ;
#16597 = DIRECTION ( 'NONE',  ( 0.000000000000000000, 0.000000000000000000, -1.000000000000000000 ) ) ;
#16598 = CARTESIAN_POINT ( 'NONE',  ( -48.99724571598702738, 77.92691374209489652, 15.00000000000006928 ) ) ;
#16599 = ORIENTED_EDGE ( 'NONE', *, *, #3641, .F. ) ;
#16600 = CARTESIAN_POINT ( 'NONE',  ( -74.72098969274614433, 107.7097065371563502, -23.55747138529295981 ) ) ;
#16601 = CARTESIAN_POINT ( 'NONE',  ( -66.14689449588691161, 109.7265287073793871, 25.00000000000000000 ) ) ;
#16602 = EDGE_LOOP ( 'NONE', ( #228, #6771, #16498, #810 ) ) ;
#16603 = CARTESIAN_POINT ( 'NONE',  ( -68.94671286412481948, 88.15687341518439268, -167.1454815528550739 ) ) ;
#16604 = DIRECTION ( 'NONE',  ( 0.000000000000000000, 0.000000000000000000, 1.000000000000000000 ) ) ;
#16605 = VERTEX_POINT ( 'NONE', #5360 ) ;
#16606 = EDGE_CURVE ( 'NONE', #13332, #6219, #8078, .T. ) ;
#16607 = CARTESIAN_POINT ( 'NONE',  ( -68.99615306438089135, 86.83301323813024908, -15.00000000000001421 ) ) ;
#16608 = CARTESIAN_POINT ( 'NONE',  ( -107.5676225674731938, 110.5691553257988460, -26.35917033480641436 ) ) ;
#16609 = VERTEX_POINT ( 'NONE', #3969 ) ;
#16610 = CARTESIAN_POINT ( 'NONE',  ( -49.26569365422058411, 90.86016871721223254, 15.00000000000006928 ) ) ;
#16611 = CARTESIAN_POINT ( 'NONE',  ( -77.40008690996572227, 78.75501449464320558, 57.36680777008252363 ) ) ;
#16612 = CARTESIAN_POINT ( 'NONE',  ( -57.08002265617300708, 84.22855780814606419, -15.00000000000001421 ) ) ;
#16613 = DIRECTION ( 'NONE',  ( 0.000000000000000000, 0.000000000000000000, 1.000000000000000000 ) ) ;
#16614 = ORIENTED_EDGE ( 'NONE', *, *, #5165, .F. ) ;
#16615 = DIRECTION ( 'NONE',  ( -1.047634945911799279E-14, 0.000000000000000000, 1.000000000000000000 ) ) ;
#16616 = CARTESIAN_POINT ( 'NONE',  ( -71.24615306438097662, 59.37761241522920841, -15.00000000000001421 ) ) ;
#16617 = SURFACE_STYLE_FILL_AREA ( #16421 ) ;
#16618 = DIRECTION ( 'NONE',  ( 0.000000000000000000, 0.000000000000000000, 1.000000000000000000 ) ) ;
#16619 = CARTESIAN_POINT ( 'NONE',  ( -21.95659417082859832, 49.25911447477409411, 27.80848509855457351 ) ) ;
#16620 = ORIENTED_EDGE ( 'NONE', *, *, #13065, .T. ) ;
#16621 = DIRECTION ( 'NONE',  ( 0.000000000000000000, 1.000000000000000000, 0.000000000000000000 ) ) ;
#16622 = CARTESIAN_POINT ( 'NONE',  ( -57.08002265617300708, 84.22855780814606419, 35.00000000000000000 ) ) ;
#16623 = ORIENTED_EDGE ( 'NONE', *, *, #10289, .F. ) ;
#16624 = LINE ( 'NONE', #3817, #7472 ) ;
#16625 =( NAMED_UNIT ( * ) SI_UNIT ( $, .STERADIAN. ) SOLID_ANGLE_UNIT ( ) );
#16626 = ORIENTED_EDGE ( 'NONE', *, *, #6068, .T. ) ;
#16627 = ORIENTED_EDGE ( 'NONE', *, *, #11562, .F. ) ;
#16628 = PLANE ( 'NONE',  #18020 ) ;
#16629 = VERTEX_POINT ( 'NONE', #16676 ) ;
#16630 = CARTESIAN_POINT ( 'NONE',  ( -64.09025127992791226, 117.8748711238780373, 35.00000000000000000 ) ) ;
#16631 = FACE_OUTER_BOUND ( 'NONE', #2818, .T. ) ;
#16632 = CARTESIAN_POINT ( 'NONE',  ( -64.58002265617299997, 84.22855780814606419, -15.00000000000001421 ) ) ;
#16633 = DIRECTION ( 'NONE',  ( -1.000000000000000000, -0.000000000000000000, -0.000000000000000000 ) ) ;
#16634 = CARTESIAN_POINT ( 'NONE',  ( -127.5926225674731995, 110.5691553257988460, -30.35917033480641081 ) ) ;
#16635 = CARTESIAN_POINT ( 'NONE',  ( -56.16856596726385220, 74.02016676429185793, 15.00000000000006928 ) ) ;
#16636 = ORIENTED_EDGE ( 'NONE', *, *, #16457, .T. ) ;
#16637 = FACE_OUTER_BOUND ( 'NONE', #1629, .T. ) ;
#16638 = CARTESIAN_POINT ( 'NONE',  ( -71.24615306438109030, 31.10327856522923540, -15.00000000000001421 ) ) ;
#16639 = ORIENTED_EDGE ( 'NONE', *, *, #15222, .F. ) ;
#16640 = ADVANCED_FACE ( 'NONE', ( #8373 ), #8470, .T. ) ;
#16641 = CARTESIAN_POINT ( 'NONE',  ( -29.09351669014244379, -91.53392936304807392, -8.561724358915437705 ) ) ;
#16642 = PLANE ( 'NONE',  #17561 ) ;
#16643 = VERTEX_POINT ( 'NONE', #4078 ) ;
#16644 = EDGE_LOOP ( 'NONE', ( #14019, #15251, #17027, #190, #17536, #2473 ) ) ;
#16645 = ORIENTED_EDGE ( 'NONE', *, *, #3208, .T. ) ;
#16646 = DIRECTION ( 'NONE',  ( 0.000000000000000000, 0.000000000000000000, 1.000000000000000000 ) ) ;
#16647 = DIRECTION ( 'NONE',  ( 0.3420201433256518375, -0.9396926207859145341, 0.000000000000000000 ) ) ;
#16648 = CARTESIAN_POINT ( 'NONE',  ( -68.99615306438086293, 92.50134268166266338, -167.1454815528550739 ) ) ;
#16649 = CARTESIAN_POINT ( 'NONE',  ( -71.24615306438076345, 119.9567435045637609, -167.1454815528550739 ) ) ;
#16650 = CARTESIAN_POINT ( 'NONE',  ( -97.59262256747319952, 54.12595869546677818, -25.00000000000000000 ) ) ;
#16651 = CARTESIAN_POINT ( 'NONE',  ( -68.99615306438097662, 61.08541618166268705, 15.00000000000006928 ) ) ;
#16652 = VERTEX_POINT ( 'NONE', #984 ) ;
#16653 = CARTESIAN_POINT ( 'NONE',  ( -66.75430539726967538, 111.9591114379528278, 24.14213053467310388 ) ) ;
#16654 = CYLINDRICAL_SURFACE ( 'NONE', #7232, 12.49999999999999645 ) ;
#16656 = ORIENTED_EDGE ( 'NONE', *, *, #2999, .T. ) ;
#16655 = CARTESIAN_POINT ( 'NONE',  ( -76.88981177685832336, 91.32863676353446181, 64.92892784414958385 ) ) ;
#16657 = CARTESIAN_POINT ( 'NONE',  ( -68.99615306438083451, 101.9261206316626698, -15.00000000000001421 ) ) ;
#16658 = DIRECTION ( 'NONE',  ( 1.000000000000000000, 0.000000000000000000, 0.000000000000000000 ) ) ;
#16659 = VECTOR ( 'NONE', #10045, 1000.000000000000000 ) ;
#16660 = VERTEX_POINT ( 'NONE', #8284 ) ;
#16661 = CARTESIAN_POINT ( 'NONE',  ( -71.24615306438070661, 137.9174286652292096, 15.00000000000006928 ) ) ;
#16662 = ORIENTED_EDGE ( 'NONE', *, *, #17180, .F. ) ;
#16663 = VERTEX_POINT ( 'NONE', #18292 ) ;
#16664 = EDGE_CURVE ( 'NONE', #11287, #4482, #17648, .T. ) ;
#16665 = FACE_OUTER_BOUND ( 'NONE', #12964, .T. ) ;
#16666 = CIRCLE ( 'NONE', #3243, 9.197489084949710403 ) ;
#16668 = EDGE_CURVE ( 'NONE', #16505, #565, #2678, .T. ) ;
#16667 = PLANE ( 'NONE',  #5189 ) ;
#16669 = CYLINDRICAL_SURFACE ( 'NONE', #8752, 20.99999999999999645 ) ;
#16670 = ORIENTED_EDGE ( 'NONE', *, *, #13978, .T. ) ;
#16671 = SHAPE_DEFINITION_REPRESENTATION ( #15525, #15553 ) ;
#16672 = CARTESIAN_POINT ( 'NONE',  ( 9.725871859128035979, 10.18744197292029519, -47.32031891155416758 ) ) ;
#16673 = CARTESIAN_POINT ( 'NONE',  ( 49.38736944425944841, -141.5628872026273086, 57.00000000000000000 ) ) ;
#16674 = ORIENTED_EDGE ( 'NONE', *, *, #10618, .T. ) ;
#16675 = DIRECTION ( 'NONE',  ( 0.000000000000000000, 0.000000000000000000, 1.000000000000000000 ) ) ;
#16676 = CARTESIAN_POINT ( 'NONE',  ( -66.51364668169601657, 56.41604328733773599, -28.00000000000000355 ) ) ;
#16677 = CARTESIAN_POINT ( 'NONE',  ( -71.24615306438097662, 60.26648315456372984, -15.00000000000001421 ) ) ;
#16678 = ADVANCED_FACE ( 'NONE', ( #6971 ), #6872, .T. ) ;
#16679 = ORIENTED_EDGE ( 'NONE', *, *, #12359, .F. ) ;
#16680 = ADVANCED_FACE ( 'NONE', ( #16971 ), #4162, .F. ) ;
#16681 = DIRECTION ( 'NONE',  ( 1.156482317317869999E-16, 0.000000000000000000, 1.000000000000000000 ) ) ;
#16682 = CARTESIAN_POINT ( 'NONE',  ( -71.24615306438094819, 69.69126110456375045, 15.00000000000006928 ) ) ;
#16683 = ORIENTED_EDGE ( 'NONE', *, *, #11477, .F. ) ;
#16684 = EDGE_CURVE ( 'NONE', #6487, #663, #17417, .T. ) ;
#16685 = DIRECTION ( 'NONE',  ( 1.000000000000000000, 0.000000000000000000, 5.551115123125786646E-16 ) ) ;
#16686 = VECTOR ( 'NONE', #13636, 1000.000000000000000 ) ;
#16687 = CARTESIAN_POINT ( 'NONE',  ( -66.28571926091831301, 56.33965956596666302, -25.37336305160129157 ) ) ;
#16688 = ORIENTED_EDGE ( 'NONE', *, *, #6885, .T. ) ;
#16689 = EDGE_CURVE ( 'NONE', #10840, #7660, #17242, .T. ) ;
#16690 = EDGE_CURVE ( 'NONE', #663, #10924, #5910, .T. ) ;
#16691 = EDGE_CURVE ( 'NONE', #5943, #4616, #8090, .T. ) ;
#16692 = CARTESIAN_POINT ( 'NONE',  ( -68.99615306438090556, 58.55867938813022988, 15.00000000000006928 ) ) ;
#16693 = VERTEX_POINT ( 'NONE', #7248 ) ;
#16694 = ADVANCED_FACE ( 'NONE', ( #12785, #8746 ), #1711, .T. ) ;
#16695 = DIRECTION ( 'NONE',  ( 0.9396926207859145341, 0.3420201433256518930, 4.890320548438480460E-16 ) ) ;
#16696 = DIRECTION ( 'NONE',  ( -0.000000000000000000, -0.000000000000000000, -1.000000000000000000 ) ) ;
#16697 = CARTESIAN_POINT ( 'NONE',  ( -68.99615306438077766, 115.1073470881302541, 15.00000000000006928 ) ) ;
#16698 = VECTOR ( 'NONE', #10413, 1000.000000000000000 ) ;
#16699 = ORIENTED_EDGE ( 'NONE', *, *, #5576, .F. ) ;
#16700 = DIRECTION ( 'NONE',  ( -0.9396926207859084279, 0.3420201433256686574, -4.890320548438448905E-16 ) ) ;
#16701 = AXIS2_PLACEMENT_3D ( 'NONE', #3889, #18215, #12518 ) ;
#16702 = DIRECTION ( 'NONE',  ( 0.000000000000000000, 1.000000000000000000, -0.000000000000000000 ) ) ;
#16703 = DIRECTION ( 'NONE',  ( 1.156482317317869999E-16, 0.000000000000000000, 1.000000000000000000 ) ) ;
#16704 = DIRECTION ( 'NONE',  ( 1.000000000000000000, 0.000000000000000000, 0.000000000000000000 ) ) ;
#16705 = LINE ( 'NONE', #7005, #10225 ) ;
#16706 = VERTEX_POINT ( 'NONE', #4610 ) ;
#16707 = EDGE_CURVE ( 'NONE', #13442, #6499, #14451, .T. ) ;
#16708 = CARTESIAN_POINT ( 'NONE',  ( -57.08002265617302839, 27.37185818390810965, 97.49999999999998579 ) ) ;
#16709 = CARTESIAN_POINT ( 'NONE',  ( -64.29464362790101006, -93.39009773859098118, 44.16867391556250766 ) ) ;
#16710 = EDGE_CURVE ( 'NONE', #4505, #13449, #11981, .T. ) ;
#16711 = FACE_OUTER_BOUND ( 'NONE', #16343, .T. ) ;
#16712 = CARTESIAN_POINT ( 'NONE',  ( -36.75995840238027768, 78.75501449464320558, 67.63319222991752611 ) ) ;
#16713 = VERTEX_POINT ( 'NONE', #302 ) ;
#16714 = CIRCLE ( 'NONE', #3278, 45.40389983439752086 ) ;
#16715 = ORIENTED_EDGE ( 'NONE', *, *, #244, .T. ) ;
#16716 = CARTESIAN_POINT ( 'NONE',  ( -63.25151023250651150, 93.09943318379590949, -167.1454815528550739 ) ) ;
#16717 = ORIENTED_EDGE ( 'NONE', *, *, #704, .T. ) ;
#16718 = DIRECTION ( 'NONE',  ( 6.950654929607132427E-15, 0.000000000000000000, -1.000000000000000000 ) ) ;
#16719 = DIRECTION ( 'NONE',  ( 0.000000000000000000, -0.8660254037844381525, 0.5000000000000008882 ) ) ;
#16720 = CARTESIAN_POINT ( 'NONE',  ( -66.33181866704592267, 58.86497344968405798, -28.00000000000000355 ) ) ;
#16721 = CARTESIAN_POINT ( 'NONE',  ( 0.05613245601037662041, 1.278525034529053306, -6.500000000000062172 ) ) ;
#16722 = DIRECTION ( 'NONE',  ( -2.062304371594500247E-16, 1.000000000000000000, 0.000000000000000000 ) ) ;
#16723 = DIRECTION ( 'NONE',  ( 1.000000000000000000, 0.000000000000000000, 5.551115123125774814E-16 ) ) ;
#16724 = ORIENTED_EDGE ( 'NONE', *, *, #12500, .F. ) ;
#16725 = AXIS2_PLACEMENT_3D ( 'NONE', #13948, #5420, #759 ) ;
#16726 = CARTESIAN_POINT ( 'NONE',  ( -70.71978124295696944, -96.08423613455721579, 5.204170427930421283E-15 ) ) ;
#16727 = AXIS2_PLACEMENT_3D ( 'NONE', #18047, #6341, #9254 ) ;
#16728 = AXIS2_PLACEMENT_3D ( 'NONE', #10191, #7300, #16063 ) ;
#16729 = DIRECTION ( 'NONE',  ( 1.000000000000000000, -0.000000000000000000, 8.326672684688672475E-15 ) ) ;
#16730 = ORIENTED_EDGE ( 'NONE', *, *, #5988, .T. ) ;
#16731 = LINE ( 'NONE', #9542, #15402 ) ;
#16732 = DIRECTION ( 'NONE',  ( 1.000000000000000000, 0.000000000000000000, 0.000000000000000000 ) ) ;
#16733 = ORIENTED_EDGE ( 'NONE', *, *, #2932, .T. ) ;
#16734 = ORIENTED_EDGE ( 'NONE', *, *, #13392, .F. ) ;
#16735 = VECTOR ( 'NONE', #15614, 1000.000000000000000 ) ;
#16736 = AXIS2_PLACEMENT_3D ( 'NONE', #13570, #16729, #15347 ) ;
#16737 = ORIENTED_EDGE ( 'NONE', *, *, #1920, .T. ) ;
#16738 = VECTOR ( 'NONE', #9150, 1000.000000000000000 ) ;
#16739 = VECTOR ( 'NONE', #17817, 1000.000000000000000 ) ;
#16740 = DIRECTION ( 'NONE',  ( -3.223492141267075737E-15, -0.000000000000000000, 1.000000000000000000 ) ) ;
#16741 = CARTESIAN_POINT ( 'NONE',  ( -57.08002265617300708, 84.22855780814606419, 77.50000000000000000 ) ) ;
#16742 = DIRECTION ( 'NONE',  ( 1.000000000000000000, 0.000000000000000000, 3.771137991253934490E-16 ) ) ;
#16743 = PRODUCT_RELATED_PRODUCT_CATEGORY ( 'part', '', ( #5524 ) ) ;
#16744 = FACE_OUTER_BOUND ( 'NONE', #6836, .T. ) ;
#16745 = CARTESIAN_POINT ( 'NONE',  ( -107.5926225674732137, 117.8748711238780373, -35.00000000000000000 ) ) ;
#16746 = DIRECTION ( 'NONE',  ( 0.000000000000000000, 0.000000000000000000, -1.000000000000000000 ) ) ;
#16747 = FACE_OUTER_BOUND ( 'NONE', #8888, .T. ) ;
#16748 = ORIENTED_EDGE ( 'NONE', *, *, #17582, .F. ) ;
#16749 = DIRECTION ( 'NONE',  ( -0.000000000000000000, -0.000000000000000000, 1.000000000000000000 ) ) ;
#16750 = FACE_OUTER_BOUND ( 'NONE', #8305, .T. ) ;
#16753 = EDGE_CURVE ( 'NONE', #9192, #850, #6941, .T. ) ;
#16752 = VERTEX_POINT ( 'NONE', #5836 ) ;
#16751 = CARTESIAN_POINT ( 'NONE',  ( -76.98508353746098010, 91.05728076224789902, 65.61100200373311964 ) ) ;
#16754 = COLOUR_RGB ( '',0.7921568627450980005, 0.8196078431372548767, 0.9333333333333333481 ) ;
#16755 = SPHERICAL_SURFACE ( 'NONE', #17705, 17.12963335357822103 ) ;
#16756 = DIRECTION ( 'NONE',  ( -0.7071067811865474617, 8.659560562354932858E-17, -0.7071067811865474617 ) ) ;
#16757 = ORIENTED_EDGE ( 'NONE', *, *, #15194, .F. ) ;
#16758 = CIRCLE ( 'NONE', #8713, 10.24900000000000055 ) ;
#16759 = VECTOR ( 'NONE', #3964, 1000.000000000000000 ) ;
#16760 = CARTESIAN_POINT ( 'NONE',  ( -47.13906347517657025, 79.99098546104539764, -167.1454815528550739 ) ) ;
#16761 = ORIENTED_EDGE ( 'NONE', *, *, #4410, .F. ) ;
#16762 = VERTEX_POINT ( 'NONE', #15840 ) ;
#16763 = AXIS2_PLACEMENT_3D ( 'NONE', #1346, #15743, #7054 ) ;
#16764 = SURFACE_SIDE_STYLE ('',( #12686 ) ) ;
#16765 = CYLINDRICAL_SURFACE ( 'NONE', #9083, 7.500000000000000000 ) ;
#16766 = DIRECTION ( 'NONE',  ( 0.9396926207859092051, 0.3420201433256663259, -1.086737899652990755E-16 ) ) ;
#16767 = ORIENTED_EDGE ( 'NONE', *, *, #15200, .F. ) ;
#16768 = SHAPE_DEFINITION_REPRESENTATION ( #4890, #14258 ) ;
#16769 = CONICAL_SURFACE ( 'NONE', #5427, 4.025000000000000355, 0.7853981633974482790 ) ;
#16770 = VECTOR ( 'NONE', #7754, 1000.000000000000000 ) ;
#16771 = CARTESIAN_POINT ( 'NONE',  ( 10.78549404122980881, 7.287009583740910124, -48.30585852359873655 ) ) ;
#16772 = DIRECTION ( 'NONE',  ( -2.062304371594500494E-16, 1.000000000000000000, -0.000000000000000000 ) ) ;
#16773 = VERTEX_POINT ( 'NONE', #17325 ) ;
#16774 = CYLINDRICAL_SURFACE ( 'NONE', #2120, 12.58237727243326987 ) ;
#16775 = CARTESIAN_POINT ( 'NONE',  ( -71.24615306438086293, 88.54081700456373483, -167.1454815528550739 ) ) ;
#16776 = DIRECTION ( 'NONE',  ( 0.000000000000000000, 0.000000000000000000, -1.000000000000000000 ) ) ;
#16777 = EDGE_CURVE ( 'NONE', #4970, #9440, #16758, .T. ) ;
#16778 = ORIENTED_EDGE ( 'NONE', *, *, #9729, .T. ) ;
#16779 = PLANE ( 'NONE',  #3874 ) ;
#16780 = LINE ( 'NONE', #15290, #8448 ) ;
#16781 = VERTEX_POINT ( 'NONE', #13130 ) ;
#16782 = AXIS2_PLACEMENT_3D ( 'NONE', #3053, #1560, #16041 ) ;
#16783 = EDGE_CURVE ( 'NONE', #7936, #17713, #3034, .T. ) ;
#16784 = LINE ( 'NONE', #16603, #8225 ) ;
#16785 = CARTESIAN_POINT ( 'NONE',  ( -66.42472841157137964, 56.38588342787130614, -27.77414277107697060 ) ) ;
#16786 = AXIS2_PLACEMENT_3D ( 'NONE', #7441, #3314, #12897 ) ;
#16787 = VECTOR ( 'NONE', #4559, 1000.000000000000000 ) ;
#16788 = EDGE_LOOP ( 'NONE', ( #3045, #3647, #7884, #9016 ) ) ;
#16789 = ORIENTED_EDGE ( 'NONE', *, *, #6879, .F. ) ;
#16790 = ORIENTED_EDGE ( 'NONE', *, *, #9703, .F. ) ;
#16791 = EDGE_CURVE ( 'NONE', #17079, #13750, #10199, .T. ) ;
#16792 = DIRECTION ( 'NONE',  ( 1.000000000000000000, 0.000000000000000000, 0.000000000000000000 ) ) ;
#16793 = PLANE ( 'NONE',  #14724 ) ;
#16794 = ADVANCED_FACE ( 'NONE', ( #14273 ), #1539, .T. ) ;
#16795 = CONICAL_SURFACE ( 'NONE', #1860, 3.445500000000021767, 0.7853981633974420618 ) ;
#16796 = ORIENTED_EDGE ( 'NONE', *, *, #8934, .F. ) ;
#16797 = DIRECTION ( 'NONE',  ( -0.000000000000000000, -0.000000000000000000, -1.000000000000000000 ) ) ;
#16798 = DIRECTION ( 'NONE',  ( -1.000000000000000000, 0.000000000000000000, 0.000000000000000000 ) ) ;
#16799 = CARTESIAN_POINT ( 'NONE',  ( -69.52933024547458274, 85.35316464920589397, -167.1454815528550739 ) ) ;
#16800 = DIRECTION ( 'NONE',  ( 1.000000000000000000, 0.000000000000000000, 5.077734830647302671E-16 ) ) ;
#16801 = ORIENTED_EDGE ( 'NONE', *, *, #11656, .T. ) ;
#16802 = DIRECTION ( 'NONE',  ( 1.156482317317869999E-16, 0.000000000000000000, 1.000000000000000000 ) ) ;
#16803 = VECTOR ( 'NONE', #8380, 1000.000000000000000 ) ;
#16804 = VECTOR ( 'NONE', #11631, 1000.000000000000000 ) ;
#16805 = CARTESIAN_POINT ( 'NONE',  ( -68.99615306438111872, 20.85956758813031797, -167.1454815528550739 ) ) ;
#16806 = DIRECTION ( 'NONE',  ( 1.156482317317869999E-16, 0.000000000000000000, 1.000000000000000000 ) ) ;
#16807 = CARTESIAN_POINT ( 'NONE',  ( -31.22998185749533206, 43.19966384034746198, -31.68386395162817237 ) ) ;
#16808 = DIRECTION ( 'NONE',  ( 0.3420201433256661594, 0.9396926207859093161, -0.000000000000000000 ) ) ;
#16809 = VERTEX_POINT ( 'NONE', #5744 ) ;
#16810 = EDGE_CURVE ( 'NONE', #16660, #13494, #9314, .T. ) ;
#16811 = ADVANCED_FACE ( 'NONE', ( #12971 ), #7342, .F. ) ;
#16812 = LINE ( 'NONE', #5587, #432 ) ;
#16813 = DIRECTION ( 'NONE',  ( 0.000000000000000000, -5.551115123125747573E-17, -1.000000000000000000 ) ) ;
#16814 = AXIS2_PLACEMENT_3D ( 'NONE', #18074, #5434, #6551 ) ;
#16815 = DIRECTION ( 'NONE',  ( 1.000000000000000000, 0.000000000000000000, 5.204170427930409450E-16 ) ) ;
#16816 = DIRECTION ( 'NONE',  ( 1.156482317317869999E-16, 0.000000000000000000, 1.000000000000000000 ) ) ;
#16817 = EDGE_LOOP ( 'NONE', ( #17792, #5544, #12824, #559 ) ) ;
#16818 = ORIENTED_EDGE ( 'NONE', *, *, #4361, .F. ) ;
#16819 = ADVANCED_FACE ( 'NONE', ( #222 ), #9107, .T. ) ;
#16820 = VECTOR ( 'NONE', #12645, 1000.000000000000000 ) ;
#16821 = VECTOR ( 'NONE', #16172, 999.9999999999998863 ) ;
#16822 = CIRCLE ( 'NONE', #8771, 4.599999999999992539 ) ;
#16823 = EDGE_CURVE ( 'NONE', #8923, #17556, #10686, .T. ) ;
#16824 = CARTESIAN_POINT ( 'NONE',  ( -46.71322837820016360, 91.21279551874765446, 15.00000000000006928 ) ) ;
#16825 = EDGE_CURVE ( 'NONE', #5132, #10461, #5061, .T. ) ;
#16826 = CARTESIAN_POINT ( 'NONE',  ( -109.6936274348538944, -91.08423613455721579, -10.65431531532595777 ) ) ;
#16827 = LINE ( 'NONE', #9915, #9653 ) ;
#16828 = ADVANCED_FACE ( 'NONE', ( #7879 ), #13594, .T. ) ;
#16829 = CARTESIAN_POINT ( 'NONE',  ( -66.40868851600845346, 56.38066346224191960, 25.00000000000000355 ) ) ;
#16830 = EDGE_LOOP ( 'NONE', ( #17602, #9346, #3177, #14851 ) ) ;
#16831 = DIRECTION ( 'NONE',  ( 0.000000000000000000, 0.000000000000000000, 1.000000000000000000 ) ) ;
#16832 = CARTESIAN_POINT ( 'NONE',  ( -57.08002265617300708, 84.22855780814606419, -167.1454815528550739 ) ) ;
#16833 = CARTESIAN_POINT ( 'NONE',  ( -57.08002265617300708, 84.22855780814606419, -167.1454815528550739 ) ) ;
#16834 = FACE_OUTER_BOUND ( 'NONE', #8033, .T. ) ;
#16835 = EDGE_LOOP ( 'NONE', ( #1741, #12819, #15380 ) ) ;
#16836 = EDGE_CURVE ( 'NONE', #14123, #14915, #3568, .T. ) ;
#16837 = AXIS2_PLACEMENT_3D ( 'NONE', #13089, #10444, #14654 ) ;
#16838 = CIRCLE ( 'NONE', #3372, 11.04359719766049430 ) ;
#16839 = AXIS2_PLACEMENT_3D ( 'NONE', #6414, #12135, #10714 ) ;
#16840 = DIRECTION ( 'NONE',  ( 1.000000000000000000, 0.000000000000000000, 3.771137991253928573E-16 ) ) ;
#16841 = ORIENTED_EDGE ( 'NONE', *, *, #2983, .F. ) ;
#16842 = LINE ( 'NONE', #18449, #3891 ) ;
#16843 = DIRECTION ( 'NONE',  ( -1.000000000000000000, -3.016910393003142859E-15, 0.000000000000000000 ) ) ;
#16844 = ORIENTED_EDGE ( 'NONE', *, *, #6514, .T. ) ;
#16845 = ORIENTED_EDGE ( 'NONE', *, *, #2403, .T. ) ;
#16846 = ORIENTED_EDGE ( 'NONE', *, *, #15764, .T. ) ;
#16847 = LINE ( 'NONE', #7200, #14689 ) ;
#16848 = AXIS2_PLACEMENT_3D ( 'NONE', #11262, #1239, #16950 ) ;
#16849 = CARTESIAN_POINT ( 'NONE',  ( -70.71978124295708312, -91.08423613455721579, 28.18308811886538479 ) ) ;
#16850 = DIRECTION ( 'NONE',  ( 1.156482317317869999E-16, 0.000000000000000000, 1.000000000000000000 ) ) ;
#16851 = DIRECTION ( 'NONE',  ( 0.9396926207859144231, 0.3420201433256520041, 4.890320548438480460E-16 ) ) ;
#16852 = CARTESIAN_POINT ( 'NONE',  ( -68.99615306438073503, 121.3905323881302962, -15.00000000000001421 ) ) ;
#16853 = LINE ( 'NONE', #9841, #12563 ) ;
#16854 = LINE ( 'NONE', #16651, #16478 ) ;
#16855 = ORIENTED_EDGE ( 'NONE', *, *, #8873, .T. ) ;
#16856 = TOROIDAL_SURFACE ( 'NONE', #3122, 7.372635429264279061, 4.962965561209096599 ) ;
#16857 = CARTESIAN_POINT ( 'NONE',  ( -86.44887054343442401, 84.22855780814606419, 37.50000000000000000 ) ) ;
#16858 = ORIENTED_EDGE ( 'NONE', *, *, #9167, .F. ) ;
#16859 = CARTESIAN_POINT ( 'NONE',  ( -45.39578445746348478, 88.67024416760654049, 15.00000000000009592 ) ) ;
#16860 = CARTESIAN_POINT ( 'NONE',  ( -62.30871503255384170, 95.58244595420320877, -167.1454815528550739 ) ) ;
#16861 = VERTEX_POINT ( 'NONE', #14703 ) ;
#16862 = SHAPE_REPRESENTATION ( '4-Bolt Mounting Plate', ( #16217 ), #3695 ) ;
#16863 = VECTOR ( 'NONE', #3443, 1000.000000000000000 ) ;
#16864 = CIRCLE ( 'NONE', #13884, 4.599999999999999645 ) ;
#16865 = FACE_OUTER_BOUND ( 'NONE', #16376, .T. ) ;
#16867 = ORIENTED_EDGE ( 'NONE', *, *, #15466, .F. ) ;
#16866 = VECTOR ( 'NONE', #11156, 1000.000000000000000 ) ;
#16868 = ORIENTED_EDGE ( 'NONE', *, *, #14644, .F. ) ;
#16869 = DIRECTION ( 'NONE',  ( 0.000000000000000000, 0.000000000000000000, 1.000000000000000000 ) ) ;
#16870 = DIRECTION ( 'NONE',  ( 0.000000000000000000, 0.000000000000000000, -1.000000000000000000 ) ) ;
#16871 = LINE ( 'NONE', #5734, #7542 ) ;
#16872 = VECTOR ( 'NONE', #18114, 1000.000000000000000 ) ;
#16873 = EDGE_LOOP ( 'NONE', ( #9267, #1815, #9300, #2591 ) ) ;
#16874 =( NAMED_UNIT ( * ) PLANE_ANGLE_UNIT ( ) SI_UNIT ( $, .RADIAN. ) );
#16875 = ORIENTED_EDGE ( 'NONE', *, *, #5273, .F. ) ;
#16876 = VECTOR ( 'NONE', #4750, 1000.000000000000000 ) ;
#16877 = AXIS2_PLACEMENT_3D ( 'NONE', #3827, #5232, #18347 ) ;
#16878 = DIRECTION ( 'NONE',  ( -0.000000000000000000, -0.000000000000000000, -1.000000000000000000 ) ) ;
#16879 = CARTESIAN_POINT ( 'NONE',  ( -97.59262256747318531, 0.3328663868096687350, -25.00000000000000000 ) ) ;
#16880 = ORIENTED_EDGE ( 'NONE', *, *, #1053, .F. ) ;
#16881 = CARTESIAN_POINT ( 'NONE',  ( -68.99615306438097662, 57.94382353166266597, -167.1454815528550739 ) ) ;
#16882 = CARTESIAN_POINT ( 'NONE',  ( -107.5926225674732137, 107.8748711238780373, -25.00000000000000000 ) ) ;
#16883 = LINE ( 'NONE', #4079, #6334 ) ;
#16884 = ORIENTED_EDGE ( 'NONE', *, *, #5375, .F. ) ;
#16885 = FACE_OUTER_BOUND ( 'NONE', #7789, .T. ) ;
#16886 = CARTESIAN_POINT ( 'NONE',  ( -68.99615306438077766, 115.1073470881302541, -15.00000000000001421 ) ) ;
#16887 = ORIENTED_EDGE ( 'NONE', *, *, #1622, .F. ) ;
#16888 = DIRECTION ( 'NONE',  ( 0.000000000000000000, 1.000000000000000000, 0.000000000000000000 ) ) ;
#16889 = EDGE_CURVE ( 'NONE', #15932, #9192, #17693, .T. ) ;
#16890 = AXIS2_PLACEMENT_3D ( 'NONE', #17498, #4679, #4759 ) ;
#16891 = CARTESIAN_POINT ( 'NONE',  ( -71.24615306438094819, 65.66079771522920794, -15.00000000000001421 ) ) ;
#16892=STYLED_ITEM('',(#18545),#12580);
#16893 = VERTEX_POINT ( 'NONE', #3382 ) ;
#16894 = AXIS2_PLACEMENT_3D ( 'NONE', #3434, #17832, #17547 ) ;
#16895 = ORIENTED_EDGE ( 'NONE', *, *, #2892, .F. ) ;
#16896 = CARTESIAN_POINT ( 'NONE',  ( -59.22941447913690638, 106.4346967249111628, 97.49999999999998579 ) ) ;
#16897 = CARTESIAN_POINT ( 'NONE',  ( -68.99615306438106188, 35.95267498166268894, -15.00000000000001421 ) ) ;
#16898 = ORIENTED_EDGE ( 'NONE', *, *, #17169, .F. ) ;
#16899 = EDGE_CURVE ( 'NONE', #15122, #10506, #16296, .T. ) ;
#16900 = DIRECTION ( 'NONE',  ( 1.000000000000000000, 0.000000000000000000, 0.000000000000000000 ) ) ;
#16901 = DIRECTION ( 'NONE',  ( 1.156482317317869999E-16, 0.000000000000000000, 1.000000000000000000 ) ) ;
#16902 = CARTESIAN_POINT ( 'NONE',  ( -21.29915789792537240, 36.55190282534568524, 35.57109117979849344 ) ) ;
#16903 = DIRECTION ( 'NONE',  ( -1.000000000000000000, 0.000000000000000000, 0.000000000000000000 ) ) ;
#16904 = ORIENTED_EDGE ( 'NONE', *, *, #8590, .F. ) ;
#16905 = PLANE ( 'NONE',  #5081 ) ;
#16906 = PLANE ( 'NONE',  #1962 ) ;
#16907 = DIRECTION ( 'NONE',  ( 0.000000000000000000, 0.000000000000000000, 1.000000000000000000 ) ) ;
#16908 = VECTOR ( 'NONE', #5583, 1000.000000000000000 ) ;
#16909 = CARTESIAN_POINT ( 'NONE',  ( -53.39175999306721110, 74.07097899412303832, -167.1454815528550739 ) ) ;
#16910 = CARTESIAN_POINT ( 'NONE',  ( -1.504738427136219414, 30.29321795796768058, 38.83614924640553312 ) ) ;
#16911 = ORIENTED_EDGE ( 'NONE', *, *, #12003, .F. ) ;
#16912 = CARTESIAN_POINT ( 'NONE',  ( -68.99615306438091977, 74.26664263813029265, 15.00000000000006928 ) ) ;
#16913 = DIRECTION ( 'NONE',  ( 0.000000000000000000, 0.000000000000000000, -1.000000000000000000 ) ) ;
#16914 = B_SPLINE_CURVE_WITH_KNOTS ( 'NONE', 3,
 ( #11002, #7079, #11295, #9978, #9695, #16687, #16980, #6882, #3978, #11199, #18303, #12705, #16785, #15489 ),
 .UNSPECIFIED., .F., .F.,
 ( 4, 2, 2, 2, 2, 2, 4 ),
 ( 0.0005070788824283136874, 0.001978938528116338819, 0.003450798173804364277, 0.004186727996648383077, 0.004922657819492402310, 0.005658587642336421544, 0.006394517465180440778 ),
 .UNSPECIFIED. ) ;
#16915 = EDGE_CURVE ( 'NONE', #16085, #6741, #9919, .T. ) ;
#16916 = CARTESIAN_POINT ( 'NONE',  ( -47.19781944808393348, 88.60139997190906058, -167.1454815528550739 ) ) ;
#16917 = PLANE ( 'NONE',  #8979 ) ;
#16918 = ORIENTED_EDGE ( 'NONE', *, *, #993, .F. ) ;
#16919 = ORIENTED_EDGE ( 'NONE', *, *, #8334, .T. ) ;
#16920 = PLANE ( 'NONE',  #395 ) ;
#16921 = ADVANCED_FACE ( 'NONE', ( #6466 ), #14800, .T. ) ;
#16922 = ADVANCED_FACE ( 'NONE', ( #7693 ), #16769, .F. ) ;
#16923 = DIRECTION ( 'NONE',  ( 1.000000000000000000, 0.000000000000000000, 0.000000000000000000 ) ) ;
#16924 = DIRECTION ( 'NONE',  ( 0.000000000000000000, 0.000000000000000000, 1.000000000000000000 ) ) ;
#16925 = CARTESIAN_POINT ( 'NONE',  ( -61.10958520376109249, -91.18731141006415442, -40.31989393471889116 ) ) ;
#16926 = EDGE_CURVE ( 'NONE', #12020, #9165, #404, .T. ) ;
#16927 = EDGE_LOOP ( 'NONE', ( #4620, #18100, #17633, #5694 ) ) ;
#16928 = ADVANCED_FACE ( 'NONE', ( #580 ), #9286, .T. ) ;
#16929 = CARTESIAN_POINT ( 'NONE',  ( -66.56703568903412815, 108.9611403144850783, -28.00000000000000355 ) ) ;
#16930 = FACE_OUTER_BOUND ( 'NONE', #4195, .T. ) ;
#16931 = DIRECTION ( 'NONE',  ( 1.000000000000000000, -0.000000000000000000, 1.047634945911800068E-14 ) ) ;
#16932 = DIRECTION ( 'NONE',  ( 0.9396926207859171987, 0.3420201433256444545, -1.086737899652999999E-16 ) ) ;
#16933 = EDGE_LOOP ( 'NONE', ( #11456, #17407, #18231, #9178 ) ) ;
#16934 = EDGE_CURVE ( 'NONE', #2433, #1839, #14976, .T. ) ;
#16935 = FACE_OUTER_BOUND ( 'NONE', #13799, .T. ) ;
#16936 = EDGE_CURVE ( 'NONE', #2809, #7618, #14979, .T. ) ;
#16937 = ORIENTED_EDGE ( 'NONE', *, *, #9063, .T. ) ;
#16938 = EDGE_CURVE ( 'NONE', #11028, #12040, #13320, .T. ) ;
#16939 = DIRECTION ( 'NONE',  ( 0.000000000000000000, -5.551115123125748189E-17, -1.000000000000000000 ) ) ;
#16940 = DIRECTION ( 'NONE',  ( -1.000000000000000000, 6.033820786006295184E-15, 0.000000000000000000 ) ) ;
#16941 = ORIENTED_EDGE ( 'NONE', *, *, #10063, .T. ) ;
#16942 = EDGE_CURVE ( 'NONE', #10632, #11429, #10219, .T. ) ;
#16943 = ORIENTED_EDGE ( 'NONE', *, *, #1140, .F. ) ;
#16944 = ORIENTED_EDGE ( 'NONE', *, *, #16130, .T. ) ;
#16945 = EDGE_CURVE ( 'NONE', #13490, #885, #6177, .T. ) ;
#16946 = EDGE_CURVE ( 'NONE', #996, #9439, #6935, .T. ) ;
#16947 = EDGE_CURVE ( 'NONE', #8038, #16154, #6847, .T. ) ;
#16948 = CARTESIAN_POINT ( 'NONE',  ( -71.24615306438096241, 57.12489050456377271, -15.00000000000001421 ) ) ;
#16949 = CARTESIAN_POINT ( 'NONE',  ( -68.99615306438089135, 67.98345733813025049, -167.1454815528550739 ) ) ;
#16950 = DIRECTION ( 'NONE',  ( 0.000000000000000000, 0.000000000000000000, 1.000000000000000000 ) ) ;
#16951 = CARTESIAN_POINT ( 'NONE',  ( -47.03642545851250389, 84.22855780814606419, -61.50000000000001421 ) ) ;
#16952 = FACE_BOUND ( 'NONE', #10658, .T. ) ;
#16953 = ORIENTED_EDGE ( 'NONE', *, *, #11231, .F. ) ;
#16954 = CARTESIAN_POINT ( 'NONE',  ( -71.24615306438114715, 10.00100075456375492, -15.00000000000001421 ) ) ;
#16955 = ORIENTED_EDGE ( 'NONE', *, *, #10945, .T. ) ;
#16956 = FACE_OUTER_BOUND ( 'NONE', #12893, .T. ) ;
#16957 = DIRECTION ( 'NONE',  ( 1.000000000000000000, 0.000000000000000000, 5.077734830647302671E-16 ) ) ;
#16958 = ORIENTED_EDGE ( 'NONE', *, *, #922, .T. ) ;
#16959 = LINE ( 'NONE', #11068, #13104 ) ;
#16960 = EDGE_CURVE ( 'NONE', #4074, #11067, #14116, .T. ) ;
#16961 = ORIENTED_EDGE ( 'NONE', *, *, #4678, .F. ) ;
#16962 = ADVANCED_FACE ( 'NONE', ( #5161 ), #12386, .F. ) ;
#16963 = VERTEX_POINT ( 'NONE', #15163 ) ;
#16964 = DIRECTION ( 'NONE',  ( 0.000000000000000000, 0.000000000000000000, 1.000000000000000000 ) ) ;
#16965 = ORIENTED_EDGE ( 'NONE', *, *, #10967, .F. ) ;
#16966 = ORIENTED_EDGE ( 'NONE', *, *, #12667, .F. ) ;
#16967 = CARTESIAN_POINT ( 'NONE',  ( -65.16279959635889441, 77.92691374209478283, 15.00000000000006928 ) ) ;
#16968 = CARTESIAN_POINT ( 'NONE',  ( -71.24615306438109030, 24.82009326522924297, -167.1454815528550739 ) ) ;
#16969 = ORIENTED_EDGE ( 'NONE', *, *, #18181, .F. ) ;
#16970 = CARTESIAN_POINT ( 'NONE',  ( -107.5926225674731853, 114.3311569208253786, 25.00000000000000000 ) ) ;
#16971 = FACE_OUTER_BOUND ( 'NONE', #16534, .T. ) ;
#16972 = CARTESIAN_POINT ( 'NONE',  ( -71.24615306438094819, 68.80239036522922902, -167.1454815528550739 ) ) ;
#16973 = EDGE_LOOP ( 'NONE', ( #3101, #11350, #15975, #10365 ) ) ;
#16974 = DIRECTION ( 'NONE',  ( 1.000000000000000000, 0.000000000000000000, 0.000000000000000000 ) ) ;
#16975 = LINE ( 'NONE', #8084, #16803 ) ;
#16976 = VERTEX_POINT ( 'NONE', #14317 ) ;
#16977 = EDGE_CURVE ( 'NONE', #16762, #11028, #17211, .T. ) ;
#16978 = CARTESIAN_POINT ( 'NONE',  ( -71.24615306438089135, 85.39922435456371375, 15.00000000000006928 ) ) ;
#16979 = ORIENTED_EDGE ( 'NONE', *, *, #13214, .T. ) ;
#16980 = CARTESIAN_POINT ( 'NONE',  ( -66.22404118522587169, 56.31946035176153487, -25.60950434884761506 ) ) ;
#16981 = VERTEX_POINT ( 'NONE', #3947 ) ;
#16982 = TOROIDAL_SURFACE ( 'NONE', #8012, 10.65431531532568243, 5.000000000000000000 ) ;
#16983 = CYLINDRICAL_SURFACE ( 'NONE', #18041, 4.599999999999999645 ) ;
#16984 = LINE ( 'NONE', #8293, #2821 ) ;
#16985 = DIRECTION ( 'NONE',  ( 0.000000000000000000, -5.551115123125748189E-17, -1.000000000000000000 ) ) ;
#16986 = ORIENTED_EDGE ( 'NONE', *, *, #14769, .F. ) ;
#16987 = B_SPLINE_CURVE_WITH_KNOTS ( 'NONE', 3,
 ( #12648, #18346, #2814, #9918, #11418, #8321, #5518, #11244, #16929, #5690, #2713, #15521, #7027, #1410 ),
 .UNSPECIFIED., .F., .F.,
 ( 4, 2, 2, 2, 2, 2, 4 ),
 ( 0.01773859478439106935, 0.01909689306834340405, 0.01977604221031956794, 0.02045519135229573529, 0.02113434049427189917, 0.02181348963624806653, 0.02317178792020043246 ),
 .UNSPECIFIED. ) ;
#16988 = DIRECTION ( 'NONE',  ( 0.9396926207859171987, 0.3420201433256445100, 4.890320548438495251E-16 ) ) ;
#16989 = DIRECTION ( 'NONE',  ( 0.000000000000000000, 1.000000000000000000, 0.000000000000000000 ) ) ;
#16990 = DIRECTION ( 'NONE',  ( 1.156482317317869999E-16, 0.000000000000000000, 1.000000000000000000 ) ) ;
#16991 = CARTESIAN_POINT ( 'NONE',  ( 4.699999999999995737, -7.505553499465293932, 1.040834085586084257E-14 ) ) ;
#16992 = ORIENTED_EDGE ( 'NONE', *, *, #5621, .F. ) ;
#16993 = EDGE_CURVE ( 'NONE', #7503, #15821, #18081, .T. ) ;
#16994 = CARTESIAN_POINT ( 'NONE',  ( 5.699999999999996625, 0.000000000000000000, 0.000000000000000000 ) ) ;
#16995 = CARTESIAN_POINT ( 'NONE',  ( -98.90286936182235422, -111.0842361345572158, -2.027180301682503564E-13 ) ) ;
#16996 = VECTOR ( 'NONE', #5795, 1000.000000000000000 ) ;
#16997 = CARTESIAN_POINT ( 'NONE',  ( -28.63941924468362998, 41.66079135237048803, -32.61277883979558823 ) ) ;
#16998 = PLANE ( 'NONE',  #11431 ) ;
#16999 = EDGE_LOOP ( 'NONE', ( #3949, #2677, #3123, #16157 ) ) ;
#17000 = FACE_OUTER_BOUND ( 'NONE', #2850, .T. ) ;
#17001 = CARTESIAN_POINT ( 'NONE',  ( -68.99615306438079188, 105.6825691381303045, -15.00000000000001421 ) ) ;
#17002 = CARTESIAN_POINT ( 'NONE',  ( -68.99615306438106188, 23.38630438166269698, -15.00000000000001421 ) ) ;
#17003 = CARTESIAN_POINT ( 'NONE',  ( -107.5926225674731853, 50.58224449241411236, 25.00000000000000000 ) ) ;
#17004 = ORIENTED_EDGE ( 'NONE', *, *, #12827, .T. ) ;
#17005 = ORIENTED_EDGE ( 'NONE', *, *, #17386, .T. ) ;
#17006 = AXIS2_PLACEMENT_3D ( 'NONE', #2880, #16901, #14106 ) ;
#17007 = CARTESIAN_POINT ( 'NONE',  ( 0.5805565836007747782, -7.505553499465293932, 1.040834085586084257E-14 ) ) ;
#17008 = ORIENTED_EDGE ( 'NONE', *, *, #12825, .F. ) ;
#17009 = CARTESIAN_POINT ( 'NONE',  ( -107.5926225674731853, 106.8071537307723133, 25.00000000000000000 ) ) ;
#17010 = CARTESIAN_POINT ( 'NONE',  ( -75.86129610575210336, 61.64996188551982925, 25.00000000000000355 ) ) ;
#17011 = CARTESIAN_POINT ( 'NONE',  ( -57.08002265617300708, 84.22855780814606419, -47.49999999999999289 ) ) ;
#17012 = VERTEX_POINT ( 'NONE', #5340 ) ;
#17013 = EDGE_CURVE ( 'NONE', #3167, #18012, #13791, .T. ) ;
#17014 = DIRECTION ( 'NONE',  ( 0.000000000000000000, 0.000000000000000000, 1.000000000000000000 ) ) ;
#17015 = DIRECTION ( 'NONE',  ( 1.156482317317869999E-16, 0.000000000000000000, 1.000000000000000000 ) ) ;
#17016 = LINE ( 'NONE', #13013, #6104 ) ;
#17017 = CARTESIAN_POINT ( 'NONE',  ( -71.24615306438086293, 94.82400230456377699, -15.00000000000001421 ) ) ;
#17018 = ORIENTED_EDGE ( 'NONE', *, *, #10300, .T. ) ;
#17019 = DIRECTION ( 'NONE',  ( 0.9396926207859110924, 0.3420201433256612189, -1.086737899652992973E-16 ) ) ;
#17020 = CIRCLE ( 'NONE', #5667, 5.654315315325682434 ) ;
#17021 = ORIENTED_EDGE ( 'NONE', *, *, #12398, .T. ) ;
#17022 = EDGE_CURVE ( 'NONE', #1931, #2889, #11423, .T. ) ;
#17023 = CARTESIAN_POINT ( 'NONE',  ( -57.08002265617300708, 84.22855780814606419, -15.00000000000001421 ) ) ;
#17024 = AXIS2_PLACEMENT_3D ( 'NONE', #5664, #11392, #4277 ) ;
#17025 = CARTESIAN_POINT ( 'NONE',  ( -70.85175816390371040, -141.5628872026273086, -57.00000000000000000 ) ) ;
#17026 = ORIENTED_EDGE ( 'NONE', *, *, #5852, .F. ) ;
#17027 = ORIENTED_EDGE ( 'NONE', *, *, #18094, .F. ) ;
#17028 = ORIENTED_EDGE ( 'NONE', *, *, #13085, .F. ) ;
#17029 = CARTESIAN_POINT ( 'NONE',  ( -68.99615306438106188, 29.66948968166269296, -167.1454815528550739 ) ) ;
#17030 = CARTESIAN_POINT ( 'NONE',  ( -107.5926225674731853, 107.8748711238780373, 25.00000000000000000 ) ) ;
#17032 = EDGE_CURVE ( 'NONE', #5963, #12287, #8055, .T. ) ;
#17031 = AXIS2_PLACEMENT_3D ( 'NONE', #7972, #9562, #1077 ) ;
#17033 = DIRECTION ( 'NONE',  ( 1.000000000000000000, 0.000000000000000000, 3.771137991253928573E-16 ) ) ;
#17034 = ADVANCED_FACE ( 'NONE', ( #13969 ), #16654, .T. ) ;
#17035 = CARTESIAN_POINT ( 'NONE',  ( -107.5676225674731654, 57.88796029049330372, -26.35917033480641436 ) ) ;
#17036 = CIRCLE ( 'NONE', #3577, 42.49926016644946003 ) ;
#17037 = DIRECTION ( 'NONE',  ( -1.000000000000000000, 0.000000000000000000, 0.000000000000000000 ) ) ;
#17038 = VECTOR ( 'NONE', #13933, 1000.000000000000000 ) ;
#17039 = EDGE_LOOP ( 'NONE', ( #5321, #14760, #591, #10677 ) ) ;
#17040 = LINE ( 'NONE', #2840, #13192 ) ;
#17041 = VERTEX_POINT ( 'NONE', #6558 ) ;
#17042 = DIRECTION ( 'NONE',  ( 0.000000000000000000, 1.779758311459927780E-16, 1.000000000000000000 ) ) ;
#17043 = DIRECTION ( 'NONE',  ( 1.156482317317869999E-16, 0.000000000000000000, 1.000000000000000000 ) ) ;
#17044 = EDGE_LOOP ( 'NONE', ( #14717, #8865, #16992, #9774 ) ) ;
#17045 = EDGE_CURVE ( 'NONE', #5342, #14885, #3763, .T. ) ;
#17046 = AXIS2_PLACEMENT_3D ( 'NONE', #1118, #16816, #9340 ) ;
#17047 = EDGE_CURVE ( 'NONE', #5572, #18030, #8162, .T. ) ;
#17048 = EDGE_CURVE ( 'NONE', #16981, #4466, #11063, .T. ) ;
#17049 = CARTESIAN_POINT ( 'NONE',  ( -112.0226416184556797, -91.42293805878655633, -8.824452519952979301 ) ) ;
#17050 = VERTEX_POINT ( 'NONE', #6761 ) ;
#17051 = AXIS2_PLACEMENT_3D ( 'NONE', #10188, #17651, #1953 ) ;
#17052 = VECTOR ( 'NONE', #8301, 1000.000000000000000 ) ;
#17053 = AXIS2_PLACEMENT_3D ( 'NONE', #2787, #16797, #12325 ) ;
#17054 = ORIENTED_EDGE ( 'NONE', *, *, #17714, .F. ) ;
#17055 = EDGE_CURVE ( 'NONE', #9789, #12932, #12479, .T. ) ;
#17056 = CARTESIAN_POINT ( 'NONE',  ( -100.4870060002411805, -151.5628872026273086, 57.00000000000000000 ) ) ;
#17057 = LINE ( 'NONE', #3201, #17986 ) ;
#17058 = VERTEX_POINT ( 'NONE', #18171 ) ;
#17059 = CONTEXT_DEPENDENT_SHAPE_REPRESENTATION ( #9693, #15381 ) ;
#17060 = CIRCLE ( 'NONE', #5409, 12.50000000000000355 ) ;
#17061 = ORIENTED_EDGE ( 'NONE', *, *, #2899, .F. ) ;
#17062 = ADVANCED_FACE ( 'NONE', ( #16750 ), #15369, .T. ) ;
#17063 = DIRECTION ( 'NONE',  ( 0.000000000000000000, 1.000000000000000000, 0.000000000000000000 ) ) ;
#17064 = EDGE_CURVE ( 'NONE', #11474, #1178, #2912, .T. ) ;
#17065 = CARTESIAN_POINT ( 'NONE',  ( -102.4618227840623774, -151.5628872026273086, -36.00000000000000000 ) ) ;
#17066 = ORIENTED_EDGE ( 'NONE', *, *, #10156, .T. ) ;
#17067 = CARTESIAN_POINT ( 'NONE',  ( -71.24615306438111872, 18.53690796522925055, -15.00000000000001421 ) ) ;
#17068 = DIRECTION ( 'NONE',  ( 0.000000000000000000, 1.000000000000000000, -0.000000000000000000 ) ) ;
#17069 = DIRECTION ( 'NONE',  ( 1.156482317317869999E-16, 0.000000000000000000, 1.000000000000000000 ) ) ;
#17070 = CIRCLE ( 'NONE', #322, 3.999999999999996447 ) ;
#17071 = VECTOR ( 'NONE', #3402, 1000.000000000000000 ) ;
#17072 = ORIENTED_EDGE ( 'NONE', *, *, #13514, .F. ) ;
#17073 = CARTESIAN_POINT ( 'NONE',  ( -70.71978124295668522, -96.08423613455721579, -28.18308811886538479 ) ) ;
#17074 = VERTEX_POINT ( 'NONE', #1493 ) ;
#17075 = EDGE_CURVE ( 'NONE', #13190, #8099, #14673, .T. ) ;
#17076 = ORIENTED_EDGE ( 'NONE', *, *, #13582, .T. ) ;
#17077 = AXIS2_PLACEMENT_3D ( 'NONE', #11707, #16003, #3188 ) ;
#17078 = LINE ( 'NONE', #1184, #2523 ) ;
#17079 = VERTEX_POINT ( 'NONE', #11598 ) ;
#17080 = VECTOR ( 'NONE', #11826, 1000.000000000000000 ) ;
#17081 = AXIS2_PLACEMENT_3D ( 'NONE', #9257, #16357, #17667 ) ;
#17082 = ORIENTED_EDGE ( 'NONE', *, *, #8936, .T. ) ;
#17083 = LINE ( 'NONE', #18410, #8494 ) ;
#17084 = ORIENTED_EDGE ( 'NONE', *, *, #4597, .F. ) ;
#17085 = CARTESIAN_POINT ( 'NONE',  ( -115.7702289486887395, -91.08423613455721579, -5.654315315326000402 ) ) ;
#17086 = CARTESIAN_POINT ( 'NONE',  ( -50.41499038512538533, 117.9449492212793444, -7.000000000000013323 ) ) ;
#17087 = LINE ( 'NONE', #14288, #2488 ) ;
#17088 = CARTESIAN_POINT ( 'NONE',  ( -68.99615306438094819, 71.12504998813029999, -167.1454815528550739 ) ) ;
#17089 = VERTEX_POINT ( 'NONE', #14403 ) ;
#17090 = VECTOR ( 'NONE', #11842, 1000.000000000000000 ) ;
#17091 = FACE_OUTER_BOUND ( 'NONE', #15922, .T. ) ;
#17092 = DIRECTION ( 'NONE',  ( -0.9396926207859069846, 0.3420201433256723766, 1.086737899652988166E-16 ) ) ;
#17093 = CARTESIAN_POINT ( 'NONE',  ( 11.11858012585388522, 6.298571833544852616, 48.62870262240658548 ) ) ;
#17094 = ORIENTED_EDGE ( 'NONE', *, *, #16710, .F. ) ;
#17095 = VECTOR ( 'NONE', #14841, 1000.000000000000000 ) ;
#17096 = VECTOR ( 'NONE', #5186, 1000.000000000000114 ) ;
#17097 = FACE_OUTER_BOUND ( 'NONE', #8899, .T. ) ;
#17098 = DIRECTION ( 'NONE',  ( 0.000000000000000000, 0.000000000000000000, 1.000000000000000000 ) ) ;
#17099 = DIRECTION ( 'NONE',  ( 1.000000000000000000, 0.000000000000000000, 0.000000000000000000 ) ) ;
#17100 = CARTESIAN_POINT ( 'NONE',  ( -53.53072411395612562, 94.43552448259771381, -15.00000000000001421 ) ) ;
#17101 = ORIENTED_EDGE ( 'NONE', *, *, #6957, .T. ) ;
#17102 = ORIENTED_EDGE ( 'NONE', *, *, #15097, .F. ) ;
#17103 = VECTOR ( 'NONE', #11551, 1000.000000000000000 ) ;
#17104 = EDGE_CURVE ( 'NONE', #15616, #14959, #6304, .T. ) ;
#17105 = ORIENTED_EDGE ( 'NONE', *, *, #7120, .F. ) ;
#17106 = VECTOR ( 'NONE', #2443, 1000.000000000000000 ) ;
#17107 = AXIS2_PLACEMENT_3D ( 'NONE', #3209, #8748, #7608 ) ;
#17108 = DIRECTION ( 'NONE',  ( -1.000000000000000000, 0.000000000000000000, 0.000000000000000000 ) ) ;
#17109 = DIRECTION ( 'NONE',  ( 1.000000000000000000, 0.000000000000000000, 0.000000000000000000 ) ) ;
#17110 = ORIENTED_EDGE ( 'NONE', *, *, #8626, .T. ) ;
#17111 = CARTESIAN_POINT ( 'NONE',  ( -68.99615306438120399, -1.746436818337276931, 15.00000000000006928 ) ) ;
#17112 = FACE_OUTER_BOUND ( 'NONE', #8856, .T. ) ;
#17113 =( LENGTH_UNIT ( ) NAMED_UNIT ( * ) SI_UNIT ( .MILLI., .METRE. ) );
#17114 = CARTESIAN_POINT ( 'NONE',  ( -71.24615306438120399, 0.5762228045637918239, 15.00000000000006928 ) ) ;
#17115 = ORIENTED_EDGE ( 'NONE', *, *, #11817, .T. ) ;
#17116 = DIRECTION ( 'NONE',  ( 0.000000000000000000, 0.000000000000000000, 1.000000000000000000 ) ) ;
#17117 = VECTOR ( 'NONE', #11854, 1000.000000000000000 ) ;
#17118 = CARTESIAN_POINT ( 'NONE',  ( -123.4618227840623632, -151.5628872026273086, 36.00000000000000711 ) ) ;
#17119 = VERTEX_POINT ( 'NONE', #11949 ) ;
#17120 = VECTOR ( 'NONE', #14510, 1000.000000000000000 ) ;
#17121 = DIRECTION ( 'NONE',  ( 1.000000000000000000, -0.000000000000000000, -0.000000000000000000 ) ) ;
#17122 = AXIS2_PLACEMENT_3D ( 'NONE', #16608, #4819, #15116 ) ;
#17123 = LINE ( 'NONE', #15734, #3532 ) ;
#17124 = ORIENTED_EDGE ( 'NONE', *, *, #13977, .F. ) ;
#17125 = ORIENTED_EDGE ( 'NONE', *, *, #14973, .F. ) ;
#17126 = VECTOR ( 'NONE', #5102, 1000.000000000000000 ) ;
#17127 = CARTESIAN_POINT ( 'NONE',  ( -71.24615306438074924, 126.2399288045637462, -15.00000000000001421 ) ) ;
#17128 = CARTESIAN_POINT ( 'NONE',  ( -71.24615306438080609, 103.3599095152292193, -15.00000000000001421 ) ) ;
#17129 = CARTESIAN_POINT ( 'NONE',  ( -70.71978124295708312, -91.08423613455721579, 28.18308811886538479 ) ) ;
#17130 = EDGE_CURVE ( 'NONE', #7016, #4262, #16160, .T. ) ;
#17131 =( GEOMETRIC_REPRESENTATION_CONTEXT ( 3 ) GLOBAL_UNCERTAINTY_ASSIGNED_CONTEXT ( ( #12837 ) ) GLOBAL_UNIT_ASSIGNED_CONTEXT ( ( #6501, #5100, #14918 ) ) REPRESENTATION_CONTEXT ( 'NONE', 'WORKASPACE' ) );
#17132 = DIRECTION ( 'NONE',  ( 0.000000000000000000, 0.000000000000000000, 1.000000000000000000 ) ) ;
#17133 = VECTOR ( 'NONE', #13142, 1000.000000000000000 ) ;
#17134 = AXIS2_PLACEMENT_3D ( 'NONE', #9726, #2900, #15328 ) ;
#17135 = DIRECTION ( 'NONE',  ( -1.047634945911799279E-14, 0.000000000000000000, 1.000000000000000000 ) ) ;
#17136 = ORIENTED_EDGE ( 'NONE', *, *, #123, .T. ) ;
#17137 = DIRECTION ( 'NONE',  ( -0.000000000000000000, 0.000000000000000000, -1.000000000000000000 ) ) ;
#17138 = VERTEX_POINT ( 'NONE', #10186 ) ;
#17139 = CARTESIAN_POINT ( 'NONE',  ( -80.72210053294904242, -91.12516209206944495, 39.81919198398647097 ) ) ;
#17140 = PLANE ( 'NONE',  #17614 ) ;
#17141 = ORIENTED_EDGE ( 'NONE', *, *, #3956, .F. ) ;
#17142 = DIRECTION ( 'NONE',  ( -1.000000000000000000, 0.000000000000000000, 0.000000000000000000 ) ) ;
#17143 = ORIENTED_EDGE ( 'NONE', *, *, #4232, .F. ) ;
#17144 = EDGE_CURVE ( 'NONE', #2191, #3839, #55, .T. ) ;
#17145 = FILL_AREA_STYLE ('',( #1324 ) ) ;
#17146 = VECTOR ( 'NONE', #1108, 1000.000000000000000 ) ;
#17147 = CIRCLE ( 'NONE', #15038, 4.999999999999998224 ) ;
#17148 = EDGE_LOOP ( 'NONE', ( #15273, #18466, #10046, #13299 ) ) ;
#17149 = CARTESIAN_POINT ( 'NONE',  ( -102.4618227840623774, -151.5628872026273086, -57.00000000000000000 ) ) ;
#17150 = DIRECTION ( 'NONE',  ( -0.9396926207859069846, 0.3420201433256723766, -4.890320548438442003E-16 ) ) ;
#17151 = DIRECTION ( 'NONE',  ( 1.000000000000000000, -0.000000000000000000, -0.000000000000000000 ) ) ;
#17152 = EDGE_CURVE ( 'NONE', #3088, #13411, #17373, .T. ) ;
#17153 = CIRCLE ( 'NONE', #1027, 26.04359719766049608 ) ;
#17154 = ORIENTED_EDGE ( 'NONE', *, *, #17540, .F. ) ;
#17155 = ITEM_DEFINED_TRANSFORMATION ( 'NONE', 'NONE', #5173,  #16217 ) ;
#17156 = EDGE_CURVE ( 'NONE', #15520, #11474, #1950, .T. ) ;
#17157 = CARTESIAN_POINT ( 'NONE',  ( -71.24615306438091977, 78.22716831522920700, -15.00000000000001421 ) ) ;
#17158 = ORIENTED_EDGE ( 'NONE', *, *, #10300, .F. ) ;
#17159 = VECTOR ( 'NONE', #10468, 1000.000000000000000 ) ;
#17160 = DIRECTION ( 'NONE',  ( 0.3420201433256507828, -0.9396926207859149782, 0.000000000000000000 ) ) ;
#17161 = EDGE_CURVE ( 'NONE', #7660, #8703, #17332, .T. ) ;
#17162 = CARTESIAN_POINT ( 'NONE',  ( -92.59262256747319952, 57.88796029049330372, -26.35917033480641436 ) ) ;
#17163 = DIRECTION ( 'NONE',  ( -1.000000000000000000, 0.000000000000000000, 0.000000000000000000 ) ) ;
#17164 = VECTOR ( 'NONE', #7376, 1000.000000000000000 ) ;
#17165 = EDGE_LOOP ( 'NONE', ( #12787, #3818, #16801, #6297 ) ) ;
#17166 = DIRECTION ( 'NONE',  ( 0.000000000000000000, 0.000000000000000000, -1.000000000000000000 ) ) ;
#17167 = ORIENTED_EDGE ( 'NONE', *, *, #12006, .T. ) ;
#17168 = ORIENTED_EDGE ( 'NONE', *, *, #16113, .F. ) ;
#17169 = EDGE_CURVE ( 'NONE', #11983, #538, #3934, .T. ) ;
#17170 = CIRCLE ( 'NONE', #9393, 4.599999999999999645 ) ;
#17171 = DIRECTION ( 'NONE',  ( 1.000000000000000000, 0.000000000000000000, 1.040834085586083310E-14 ) ) ;
#17172 = EDGE_CURVE ( 'NONE', #13472, #15291, #8106, .T. ) ;
#17173 = EDGE_CURVE ( 'NONE', #18159, #9136, #4937, .T. ) ;
#17174 = VECTOR ( 'NONE', #16317, 1000.000000000000000 ) ;
#17175 = VECTOR ( 'NONE', #1090, 1000.000000000000000 ) ;
#17176 = DIRECTION ( 'NONE',  ( 0.000000000000000000, 0.000000000000000000, 1.000000000000000000 ) ) ;
#17177 = LINE ( 'NONE', #4364, #15941 ) ;
#17178 = EDGE_CURVE ( 'NONE', #4, #18453, #3056, .T. ) ;
#17179 = EDGE_LOOP ( 'NONE', ( #16953, #16261, #15765, #12350 ) ) ;
#17180 = EDGE_CURVE ( 'NONE', #9602, #10794, #12317, .T. ) ;
#17181 = CARTESIAN_POINT ( 'NONE',  ( -66.27474722583565381, 78.55081803573735044, -167.1454815528550739 ) ) ;
#17182 = CYLINDRICAL_SURFACE ( 'NONE', #9229, 11.04359719766049430 ) ;
#17183 = LINE ( 'NONE', #16799, #635 ) ;
#17184 = CARTESIAN_POINT ( 'NONE',  ( 276.3098885457529832, -32.62665103886256190, -7.000000000000010658 ) ) ;
#17185 = ORIENTED_EDGE ( 'NONE', *, *, #11126, .F. ) ;
#17186 = LINE ( 'NONE', #17346, #7496 ) ;
#17187 = CARTESIAN_POINT ( 'NONE',  ( -127.5926225674732279, 47.87487112387803023, 15.00000000000004263 ) ) ;
#17188 = LINE ( 'NONE', #6023, #8124 ) ;
#17189 = ORIENTED_EDGE ( 'NONE', *, *, #4922, .F. ) ;
#17190 = AXIS2_PLACEMENT_3D ( 'NONE', #14688, #9183, #17577 ) ;
#17191 = VECTOR ( 'NONE', #9176, 1000.000000000000000 ) ;
#17192 = VECTOR ( 'NONE', #6214, 1000.000000000000000 ) ;
#17193 = DIRECTION ( 'NONE',  ( -5.204170427930409450E-16, 0.000000000000000000, 1.000000000000000000 ) ) ;
#17194 = FACE_OUTER_BOUND ( 'NONE', #13548, .T. ) ;
#17195 = LINE ( 'NONE', #14023, #9884 ) ;
#17196 = EDGE_LOOP ( 'NONE', ( #9039, #18061, #11924, #6146 ) ) ;
#17197 = EDGE_CURVE ( 'NONE', #3821, #14173, #10647, .T. ) ;
#17198 = VERTEX_POINT ( 'NONE', #8013 ) ;
#17199 = CARTESIAN_POINT ( 'NONE',  ( -123.4618227840623632, -151.5628872026273086, -35.99999999999997158 ) ) ;
#17200 = CARTESIAN_POINT ( 'NONE',  ( 0.000000000000000000, 0.000000000000000000, 0.000000000000000000 ) ) ;
#17201 = CIRCLE ( 'NONE', #465, 4.599999999999992539 ) ;
#17202 = APPLICATION_CONTEXT ( 'automotive_design' ) ;
#17203 = CARTESIAN_POINT ( 'NONE',  ( -67.59262256747315689, 111.6514400295689313, 15.00000000000006040 ) ) ;
#17204 = CARTESIAN_POINT ( 'NONE',  ( 4.699999999999995737, 6.499999999999901412, 2.428612866367529932E-14 ) ) ;
#17205 = ORIENTED_EDGE ( 'NONE', *, *, #14790, .F. ) ;
#17206 = DIRECTION ( 'NONE',  ( 0.000000000000000000, 0.000000000000000000, 1.000000000000000000 ) ) ;
#17207 = CARTESIAN_POINT ( 'NONE',  ( -50.90853507983961634, 93.09943318379598054, -15.00000000000001421 ) ) ;
#17208 = CARTESIAN_POINT ( 'NONE',  ( -194.4437806548868934, -151.5628872026273086, 18.23991632971911869 ) ) ;
#17209 = DIRECTION ( 'NONE',  ( -1.000000000000000000, -2.062304371594500247E-16, -0.000000000000000000 ) ) ;
#17210 = ORIENTED_EDGE ( 'NONE', *, *, #5712, .T. ) ;
#17211 = LINE ( 'NONE', #6664, #14098 ) ;
#17212 = DIRECTION ( 'NONE',  ( 0.000000000000000000, 0.000000000000000000, 1.000000000000000000 ) ) ;
#17213 = ORIENTED_EDGE ( 'NONE', *, *, #14638, .F. ) ;
#17214 = DIRECTION ( 'NONE',  ( 1.000000000000000000, 0.000000000000000000, 0.000000000000000000 ) ) ;
#17215 = DIRECTION ( 'NONE',  ( 0.000000000000000000, 0.000000000000000000, 1.000000000000000000 ) ) ;
#17216 = EDGE_LOOP ( 'NONE', ( #12154, #12692, #1577, #11757 ) ) ;
#17217 = ORIENTED_EDGE ( 'NONE', *, *, #18461, .T. ) ;
#17218 = LINE ( 'NONE', #10113, #9699 ) ;
#17219 = DIRECTION ( 'NONE',  ( 0.9396926207859084279, 0.3420201433256686574, -1.086737899652989892E-16 ) ) ;
#17220 = DIRECTION ( 'NONE',  ( 0.000000000000000000, 0.000000000000000000, 1.000000000000000000 ) ) ;
#17221 = DIRECTION ( 'NONE',  ( 0.000000000000000000, 0.000000000000000000, 1.000000000000000000 ) ) ;
#17222 = CARTESIAN_POINT ( 'NONE',  ( -71.24615306438089135, 82.25763170456374951, -15.00000000000001421 ) ) ;
#17223 = ORIENTED_EDGE ( 'NONE', *, *, #4684, .F. ) ;
#17224 = EDGE_CURVE ( 'NONE', #2102, #8537, #6610, .T. ) ;
#17225 = DIRECTION ( 'NONE',  ( 1.000000000000000000, 0.000000000000000000, 0.000000000000000000 ) ) ;
#17226 = ORIENTED_EDGE ( 'NONE', *, *, #15148, .F. ) ;
#17227 = DIRECTION ( 'NONE',  ( -1.000000000000000000, 0.000000000000000000, 1.387778780781446662E-16 ) ) ;
#17228 = CARTESIAN_POINT ( 'NONE',  ( -198.5768363665157494, 84.22855780814606419, 62.50000000000001421 ) ) ;
#17229 = ORIENTED_EDGE ( 'NONE', *, *, #2421, .F. ) ;
#17230 = CARTESIAN_POINT ( 'NONE',  ( -71.24615306438079188, 113.6735582045637045, 15.00000000000006928 ) ) ;
#17231 = EDGE_LOOP ( 'NONE', ( #9317, #4454, #12485, #11241, #1040, #5770, #12805 ) ) ;
#17232 = VERTEX_POINT ( 'NONE', #823 ) ;
#17233 = B_SPLINE_CURVE_WITH_KNOTS ( 'NONE', 3,
 ( #9374, #13678, #17972, #9103, #17791, #7875 ),
 .UNSPECIFIED., .F., .F.,
 ( 4, 2, 4 ),
 ( 2.380733002060942798E-07, 0.001898835937927345141, 0.003797433802554483605 ),
 .UNSPECIFIED. ) ;
#17234 = CARTESIAN_POINT ( 'NONE',  ( -71.24615306438082030, 82.25763170456377793, 15.00000000000006928 ) ) ;
#17235 = B_SPLINE_CURVE_WITH_KNOTS ( 'NONE', 3,
 ( #10172, #7192, #2979, #1749, #13175, #4647, #11766, #8685, #11590, #15622, #8521, #11415, #10011, #2902 ),
 .UNSPECIFIED., .F., .F.,
 ( 4, 2, 2, 2, 2, 2, 4 ),
 ( 0.0006178928065812205276, 0.001352643563036826091, 0.002087394319492431871, 0.002822145075948037651, 0.003556895832403643432, 0.005026397345314864533, 0.006495898858226086502 ),
 .UNSPECIFIED. ) ;
#17236 = DIRECTION ( 'NONE',  ( -0.000000000000000000, -1.000000000000000000, -0.000000000000000000 ) ) ;
#17237 = DIRECTION ( 'NONE',  ( -0.9396926207859084279, 0.3420201433256686574, 0.000000000000000000 ) ) ;
#17238 = VERTEX_POINT ( 'NONE', #632 ) ;
#17239 = ITEM_DEFINED_TRANSFORMATION ( 'NONE', 'NONE', #17423,  #16217 ) ;
#17240 = VERTEX_POINT ( 'NONE', #7935 ) ;
#17241 = DIRECTION ( 'NONE',  ( 0.000000000000000000, 1.000000000000000000, 0.000000000000000000 ) ) ;
#17242 = LINE ( 'NONE', #10330, #11686 ) ;
#17243 = EDGE_CURVE ( 'NONE', #626, #10454, #3521, .T. ) ;
#17244 = CARTESIAN_POINT ( 'NONE',  ( 15.23320273812466041, 0.000000000000000000, 3.000000000000000000 ) ) ;
#17245 = ORIENTED_EDGE ( 'NONE', *, *, #17965, .T. ) ;
#17246 = LINE ( 'NONE', #7156, #10441 ) ;
#17247 = VERTEX_POINT ( 'NONE', #12336 ) ;
#17248 = ORIENTED_EDGE ( 'NONE', *, *, #14201, .T. ) ;
#17249 = EDGE_CURVE ( 'NONE', #5018, #7663, #9235, .T. ) ;
#17250 = ORIENTED_EDGE ( 'NONE', *, *, #14847, .F. ) ;
#17251 = DIRECTION ( 'NONE',  ( 0.000000000000000000, 0.000000000000000000, 1.000000000000000000 ) ) ;
#17252 = CARTESIAN_POINT ( 'NONE',  ( 4.699999999999995737, -7.505553499465293932, 1.040834085586084257E-14 ) ) ;
#17253 = DIRECTION ( 'NONE',  ( -0.000000000000000000, -0.000000000000000000, 1.000000000000000000 ) ) ;
#17254 = VERTEX_POINT ( 'NONE', #3438 ) ;
#17255 = ADVANCED_FACE ( 'NONE', ( #10727 ), #18029, .T. ) ;
#17256 = FACE_OUTER_BOUND ( 'NONE', #5797, .T. ) ;
#17257 = DIRECTION ( 'NONE',  ( 0.000000000000000000, 0.000000000000000000, 1.000000000000000000 ) ) ;
#17258 = DIRECTION ( 'NONE',  ( 0.000000000000000000, 0.000000000000000000, 1.000000000000000000 ) ) ;
#17259 = EDGE_CURVE ( 'NONE', #15989, #7936, #9154, .T. ) ;
#17260 = CARTESIAN_POINT ( 'NONE',  ( -76.37409655828280108, -96.08423613455721579, 45.05044770573179846 ) ) ;
#17261 = ORIENTED_EDGE ( 'NONE', *, *, #13066, .F. ) ;
#17262 = EDGE_CURVE ( 'NONE', #16485, #1951, #4538, .T. ) ;
#17263 = CARTESIAN_POINT ( 'NONE',  ( -68.99615306438074924, 120.7756765316626542, -167.1454815528550739 ) ) ;
#17264 = DIRECTION ( 'NONE',  ( 1.000000000000000000, 0.000000000000000000, 3.771137991253928573E-16 ) ) ;
#17265 = DIRECTION ( 'NONE',  ( -0.9475106458593564041, -0.3197242186372270534, 0.000000000000000000 ) ) ;
#17266 = ORIENTED_EDGE ( 'NONE', *, *, #12248, .T. ) ;
#17267 = LINE ( 'NONE', #10162, #5214 ) ;
#17268 = CIRCLE ( 'NONE', #15175, 7.500000000000007105 ) ;
#17269 = EDGE_CURVE ( 'NONE', #7354, #9885, #5444, .T. ) ;
#17270 = EDGE_CURVE ( 'NONE', #9440, #2884, #7828, .T. ) ;
#17271 = DIRECTION ( 'NONE',  ( 0.000000000000000000, 1.000000000000000000, 0.000000000000000000 ) ) ;
#17272 = EDGE_CURVE ( 'NONE', #18002, #5917, #12229, .T. ) ;
#17273 = ORIENTED_EDGE ( 'NONE', *, *, #8000, .T. ) ;
#17274 = EDGE_LOOP ( 'NONE', ( #17668, #16918, #3693, #2823 ) ) ;
#17275 = EDGE_CURVE ( 'NONE', #9163, #11177, #18485, .T. ) ;
#17276 = EDGE_CURVE ( 'NONE', #4288, #6911, #1202, .T. ) ;
#17277 = DIRECTION ( 'NONE',  ( 1.000000000000000000, 0.000000000000000000, 0.000000000000000000 ) ) ;
#17278 = CYLINDRICAL_SURFACE ( 'NONE', #7045, 4.599999999999999645 ) ;
#17279 =( NAMED_UNIT ( * ) SI_UNIT ( $, .STERADIAN. ) SOLID_ANGLE_UNIT ( ) );
#17280 = PLANE ( 'NONE',  #11742 ) ;
#17281 = FACE_OUTER_BOUND ( 'NONE', #7617, .T. ) ;
#17282 = ORIENTED_EDGE ( 'NONE', *, *, #13245, .T. ) ;
#17283 = DIRECTION ( 'NONE',  ( -0.000000000000000000, -0.000000000000000000, 1.000000000000000000 ) ) ;
#17284 = LINE ( 'NONE', #8528, #11823 ) ;
#17285 = ADVANCED_FACE ( 'NONE', ( #2607 ), #14212, .F. ) ;
#17286 = DIRECTION ( 'NONE',  ( 1.047634945911800068E-14, 0.000000000000000000, -1.000000000000000000 ) ) ;
#17287 = CARTESIAN_POINT ( 'NONE',  ( -57.08002265617300708, 84.22855780814606419, 15.00000000000006928 ) ) ;
#17288 = ORIENTED_EDGE ( 'NONE', *, *, #6287, .F. ) ;
#17289 = ADVANCED_FACE ( 'NONE', ( #5494 ), #2796, .T. ) ;
#17290 = CARTESIAN_POINT ( 'NONE',  ( -57.08002265617300708, 84.22855780814606419, -47.50000000000000000 ) ) ;
#17291 = LINE ( 'NONE', #14137, #6276 ) ;
#17292 = ORIENTED_EDGE ( 'NONE', *, *, #11562, .T. ) ;
#17293 = FACE_OUTER_BOUND ( 'NONE', #3260, .T. ) ;
#17294 = DIRECTION ( 'NONE',  ( 0.000000000000000000, 0.000000000000000000, 1.000000000000000000 ) ) ;
#17295 = ORIENTED_EDGE ( 'NONE', *, *, #931, .T. ) ;
#17296 = AXIS2_PLACEMENT_3D ( 'NONE', #5927, #323, #421 ) ;
#17297 = VERTEX_POINT ( 'NONE', #9805 ) ;
#17298 = ORIENTED_EDGE ( 'NONE', *, *, #440, .F. ) ;
#17299 = CARTESIAN_POINT ( 'NONE',  ( 0.4033376246892568795, 4.059728990630770085, 5.968343123267169759 ) ) ;
#17300 = CARTESIAN_POINT ( 'NONE',  ( 0.4037800551814316186, -4.058962678540228630, 5.969670414742723530 ) ) ;
#17301 = DIRECTION ( 'NONE',  ( -0.000000000000000000, -0.000000000000000000, 1.000000000000000000 ) ) ;
#17302 = FACE_OUTER_BOUND ( 'NONE', #18380, .T. ) ;
#17303 = DIRECTION ( 'NONE',  ( 1.000000000000000000, 0.000000000000000000, 0.000000000000000000 ) ) ;
#17304 = VERTEX_POINT ( 'NONE', #18503 ) ;
#17305 = AXIS2_PLACEMENT_3D ( 'NONE', #3212, #17798, #9017 ) ;
#17306 = DIRECTION ( 'NONE',  ( 0.000000000000000000, 0.000000000000000000, 1.000000000000000000 ) ) ;
#17307 = PLANE ( 'NONE',  #3363 ) ;
#17308 = VECTOR ( 'NONE', #4969, 1000.000000000000000 ) ;
#17309 = LINE ( 'NONE', #8450, #5363 ) ;
#17310 = ORIENTED_EDGE ( 'NONE', *, *, #4315, .T. ) ;
#17311 = DIRECTION ( 'NONE',  ( 1.000000000000000000, 0.000000000000000000, 0.000000000000000000 ) ) ;
#17312 = CYLINDRICAL_SURFACE ( 'NONE', #16068, 12.50000000000000355 ) ;
#17313 = ORIENTED_EDGE ( 'NONE', *, *, #12602, .T. ) ;
#17314 = VECTOR ( 'NONE', #387, 1000.000000000000000 ) ;
#17315 = EDGE_CURVE ( 'NONE', #17987, #2873, #16705, .T. ) ;
#17316 = VERTEX_POINT ( 'NONE', #15706 ) ;
#17317 = AXIS2_PLACEMENT_3D ( 'NONE', #9081, #4583, #13372 ) ;
#17318 = LINE ( 'NONE', #11818, #18057 ) ;
#17319 = CARTESIAN_POINT ( 'NONE',  ( -67.59262256747315689, 56.80567558672318285, 15.00000000000006928 ) ) ;
#17320 = DIRECTION ( 'NONE',  ( 0.000000000000000000, 0.000000000000000000, 1.000000000000000000 ) ) ;
#17321 = ORIENTED_EDGE ( 'NONE', *, *, #14997, .T. ) ;
#17322 = ADVANCED_FACE ( 'NONE', ( #2505 ), #7095, .T. ) ;
#17323 = ORIENTED_EDGE ( 'NONE', *, *, #11920, .T. ) ;
#17324 = DIRECTION ( 'NONE',  ( 1.000000000000000000, 0.000000000000000000, 3.223492141267071398E-15 ) ) ;
#17325 = CARTESIAN_POINT ( 'NONE',  ( -67.26033723204500347, 83.04399200740374454, 15.00000000000006928 ) ) ;
#17326 = CARTESIAN_POINT ( 'NONE',  ( -107.5926225674732137, 107.8748711238780373, -35.00000000000000000 ) ) ;
#17327 = LINE ( 'NONE', #10231, #15916 ) ;
#17328 = ORIENTED_EDGE ( 'NONE', *, *, #3441, .F. ) ;
#17329 = AXIS2_PLACEMENT_3D ( 'NONE', #13647, #17926, #5218 ) ;
#17330 = FACE_OUTER_BOUND ( 'NONE', #16553, .T. ) ;
#17331 = ORIENTED_EDGE ( 'NONE', *, *, #362, .F. ) ;
#17332 = B_SPLINE_CURVE_WITH_KNOTS ( 'NONE', 3,
 ( #4656, #13358, #534, #1583, #7559, #14663, #15887, #13184, #17646, #13273, #10105, #11861, #17551, #3077, #15804, #2990, #4733, #7295, #4472, #8793, #1676, #5960, #4560, #7382, #13097, #11683, #358, #10278, #15983, #3172, #8883, #14576, #10453, #16148, #7464, #1758, #3339, #6047, #11774, #17471, #16060, #8969, #9064, #14751 ),
 .UNSPECIFIED., .F., .F.,
 ( 4, 2, 2, 2, 2, 2, 2, 2, 2, 2, 2, 2, 2, 2, 2, 2, 2, 2, 2, 2, 2, 4 ),
 ( 0.02364448373982099005, 0.02438320150779624967, 0.02512191927577150929, 0.02659935481172202160, 0.02807679034767253390, 0.02955422588362304273, 0.03103166141957355503, 0.03177037918754881812, 0.03250909695552409162, 0.03398653249147459698, 0.03546396802742510235, 0.03694140356337561465, 0.03768012133135086733, 0.03841883909932612695, 0.03915755686730137963, 0.03989627463527663231, 0.04137371017122716543, 0.04285114570717769855, 0.04432858124312823167, 0.04506729901110349823, 0.04580601677907876479, 0.04728345231502934648 ),
 .UNSPECIFIED. ) ;
#17333 = EDGE_LOOP ( 'NONE', ( #8444, #8169, #17552, #3132 ) ) ;
#17334 = CIRCLE ( 'NONE', #1224, 7.500000000000000000 ) ;
#17335 = ORIENTED_EDGE ( 'NONE', *, *, #5847, .F. ) ;
#17336 = VECTOR ( 'NONE', #8800, 1000.000000000000000 ) ;
#17337 = VECTOR ( 'NONE', #2697, 1000.000000000000000 ) ;
#17338 = DIRECTION ( 'NONE',  ( 0.9396926207859157554, 0.3420201433256481738, 4.890320548438487362E-16 ) ) ;
#17339 = ORIENTED_EDGE ( 'NONE', *, *, #993, .T. ) ;
#17340 = DIRECTION ( 'NONE',  ( 0.000000000000000000, 0.000000000000000000, -1.000000000000000000 ) ) ;
#17341 = LINE ( 'NONE', #1553, #18203 ) ;
#17342 = LINE ( 'NONE', #12988, #9003 ) ;
#17343 = DIRECTION ( 'NONE',  ( -1.000000000000000000, -0.000000000000000000, -0.000000000000000000 ) ) ;
#17344 = ORIENTED_EDGE ( 'NONE', *, *, #7352, .T. ) ;
#17345 = ADVANCED_FACE ( 'NONE', ( #13929 ), #15505, .T. ) ;
#17346 = CARTESIAN_POINT ( 'NONE',  ( -71.24615306438094819, 66.54966845456371516, -167.1454815528550739 ) ) ;
#17347 = DIRECTION ( 'NONE',  ( -5.204170427930409450E-16, 0.000000000000000000, 1.000000000000000000 ) ) ;
#17348 = DIRECTION ( 'NONE',  ( -0.000000000000000000, -0.000000000000000000, 1.000000000000000000 ) ) ;
#17349 = ORIENTED_EDGE ( 'NONE', *, *, #5617, .T. ) ;
#17350 = VECTOR ( 'NONE', #3127, 1000.000000000000000 ) ;
#17351 = CARTESIAN_POINT ( 'NONE',  ( -71.24615306438091977, 75.08557566522922855, -167.1454815528550739 ) ) ;
#17352 = CARTESIAN_POINT ( 'NONE',  ( -64.50972932340006594, 92.07579602767982863, -167.1454815528550739 ) ) ;
#17353 = AXIS2_PLACEMENT_3D ( 'NONE', #13919, #1107, #11110 ) ;
#17354 = ORIENTED_EDGE ( 'NONE', *, *, #12608, .F. ) ;
#17355 = ADVANCED_FACE ( 'NONE', ( #8588 ), #2694, .T. ) ;
#17356 = ORIENTED_EDGE ( 'NONE', *, *, #9161, .F. ) ;
#17357 = ADVANCED_FACE ( 'NONE', ( #8403 ), #4187, .T. ) ;
#17358 = ORIENTED_EDGE ( 'NONE', *, *, #5610, .F. ) ;
#17359 = LINE ( 'NONE', #1571, #4572 ) ;
#17360 = CIRCLE ( 'NONE', #8430, 4.599999999999992539 ) ;
#17361 = DIRECTION ( 'NONE',  ( 1.000000000000000000, 0.000000000000000000, 0.000000000000000000 ) ) ;
#17362 = CARTESIAN_POINT ( 'NONE',  ( -67.59262256747317110, 57.88796029049329661, 30.35917033480639660 ) ) ;
#17363 = CARTESIAN_POINT ( 'NONE',  ( -68.99615306438111872, 14.57638228813026871, -15.00000000000001421 ) ) ;
#17364 = VERTEX_POINT ( 'NONE', #5585 ) ;
#17365 = ADVANCED_FACE ( 'NONE', ( #11400 ), #16998, .T. ) ;
#17366 = EDGE_CURVE ( 'NONE', #4896, #10257, #14727, .T. ) ;
#17367 = DIRECTION ( 'NONE',  ( -0.000000000000000000, -0.000000000000000000, -1.000000000000000000 ) ) ;
#17368 = AXIS2_PLACEMENT_3D ( 'NONE', #17877, #10493, #12186 ) ;
#17369 = AXIS2_PLACEMENT_3D ( 'NONE', #13111, #17489, #11705 ) ;
#17370 = CARTESIAN_POINT ( 'NONE',  ( -68.99615306438083451, 99.39938383813029077, -167.1454815528550739 ) ) ;
#17371 = CARTESIAN_POINT ( 'NONE',  ( 98.04320049944426785, 84.22855780814606419, 62.50000000000001421 ) ) ;
#17372 = CARTESIAN_POINT ( 'NONE',  ( 0.5805565836007609004, 3.752776749732435135, 6.499999999999981348 ) ) ;
#17373 = LINE ( 'NONE', #7652, #12917 ) ;
#17374 = FACE_BOUND ( 'NONE', #12505, .T. ) ;
#17375 = ORIENTED_EDGE ( 'NONE', *, *, #1762, .F. ) ;
#17376 = EDGE_CURVE ( 'NONE', #17860, #3439, #69, .T. ) ;
#17377 = AXIS2_PLACEMENT_3D ( 'NONE', #12013, #6386, #11917 ) ;
#17378 = DIRECTION ( 'NONE',  ( 0.3420201433256689905, 0.9396926207859084279, -0.000000000000000000 ) ) ;
#17379 = DIRECTION ( 'NONE',  ( 1.156482317317869999E-16, 0.000000000000000000, 1.000000000000000000 ) ) ;
#17380 = ORIENTED_EDGE ( 'NONE', *, *, #16132, .T. ) ;
#17381 = EDGE_CURVE ( 'NONE', #8404, #3000, #9038, .T. ) ;
#17382 = ORIENTED_EDGE ( 'NONE', *, *, #440, .T. ) ;
#17383 = VECTOR ( 'NONE', #5861, 1000.000000000000000 ) ;
#17384 = VECTOR ( 'NONE', #8032, 1000.000000000000000 ) ;
#17385 = EDGE_CURVE ( 'NONE', #9318, #6499, #11843, .T. ) ;
#17386 = EDGE_CURVE ( 'NONE', #13818, #18509, #17188, .T. ) ;
#17387 = VERTEX_POINT ( 'NONE', #11495 ) ;
#17388 = CARTESIAN_POINT ( 'NONE',  ( -57.08002265617300708, 84.22855780814606419, -15.00000000000001421 ) ) ;
#17389 = CARTESIAN_POINT ( 'NONE',  ( -71.24615306438097662, 62.51920506522922949, -15.00000000000001421 ) ) ;
#17390 = DIRECTION ( 'NONE',  ( 0.3420201433256649937, 0.9396926207859097602, -0.000000000000000000 ) ) ;
#17391 = FACE_OUTER_BOUND ( 'NONE', #6560, .T. ) ;
#17392 = EDGE_CURVE ( 'NONE', #12093, #15619, #15779, .T. ) ;
#17393 = VECTOR ( 'NONE', #15094, 1000.000000000000114 ) ;
#17394 = CARTESIAN_POINT ( 'NONE',  ( -71.24615306438100504, 49.95283446522918780, -167.1454815528550739 ) ) ;
#17395 = DIRECTION ( 'NONE',  ( 1.000000000000000000, 0.000000000000000000, 0.000000000000000000 ) ) ;
#17396 = VERTEX_POINT ( 'NONE', #4536 ) ;
#17397 = CYLINDRICAL_SURFACE ( 'NONE', #51, 12.50000000000001066 ) ;
#17398 = DIRECTION ( 'NONE',  ( 0.000000000000000000, 1.000000000000000000, 0.000000000000000000 ) ) ;
#17399 = CIRCLE ( 'NONE', #14699, 4.600000000000013856 ) ;
#17400 = AXIS2_PLACEMENT_3D ( 'NONE', #5466, #16776, #13996 ) ;
#17401 = CARTESIAN_POINT ( 'NONE',  ( -92.59262256747321373, 110.5691553257988460, 30.35917033480641081 ) ) ;
#17402 = ORIENTED_EDGE ( 'NONE', *, *, #3791, .T. ) ;
#17403 = CARTESIAN_POINT ( 'NONE',  ( -71.24615306438069240, 123.0983361545637393, 15.00000000000006928 ) ) ;
#17404 = DIRECTION ( 'NONE',  ( 0.000000000000000000, 0.000000000000000000, 1.000000000000000000 ) ) ;
#17405 = VERTEX_POINT ( 'NONE', #10255 ) ;
#17406 = CONICAL_SURFACE ( 'NONE', #1584, 6.500000000000039968, 1.047197551196600296 ) ;
#17407 = ORIENTED_EDGE ( 'NONE', *, *, #7443, .T. ) ;
#17408 = CIRCLE ( 'NONE', #1313, 11.04359719766049430 ) ;
#17409 = TOROIDAL_SURFACE ( 'NONE', #13537, 47.49926016644912607, 5.000000000000000000 ) ;
#17410 = AXIS2_PLACEMENT_3D ( 'NONE', #11588, #10266, #3163 ) ;
#17411 = DIRECTION ( 'NONE',  ( -0.9396926207859022107, 0.3420201433256853663, 1.086737899652982620E-16 ) ) ;
#17412 = CARTESIAN_POINT ( 'NONE',  ( 4.699999999999995737, 6.499999999999901412, 2.428612866367529932E-14 ) ) ;
#17413 = DIRECTION ( 'NONE',  ( 0.000000000000000000, 0.000000000000000000, 1.000000000000000000 ) ) ;
#17414 = ORIENTED_EDGE ( 'NONE', *, *, #5626, .T. ) ;
#17415 = ORIENTED_EDGE ( 'NONE', *, *, #9217, .F. ) ;
#17416 = LINE ( 'NONE', #10685, #16143 ) ;
#17417 = LINE ( 'NONE', #15674, #9301 ) ;
#17418 = CARTESIAN_POINT ( 'NONE',  ( -68.99615306438077766, 123.9172691816626610, -167.1454815528550739 ) ) ;
#17419 = DIRECTION ( 'NONE',  ( 0.000000000000000000, 1.000000000000000000, -0.000000000000000000 ) ) ;
#17420 = EDGE_LOOP ( 'NONE', ( #16645, #8696, #4381, #6353, #7554 ) ) ;
#17421 = CYLINDRICAL_SURFACE ( 'NONE', #1496, 4.599999999999999645 ) ;
#17422 = ORIENTED_EDGE ( 'NONE', *, *, #17487, .F. ) ;
#17423 = AXIS2_PLACEMENT_3D ( 'NONE', #11671, #7455, #17361 ) ;
#17424 = VECTOR ( 'NONE', #7921, 999.9999999999998863 ) ;
#17425 = LINE ( 'NONE', #14619, #12589 ) ;
#17427 = ORIENTED_EDGE ( 'NONE', *, *, #7769, .T. ) ;
#17426 = AXIS2_PLACEMENT_3D ( 'NONE', #3775, #6678, #15566 ) ;
#17428 = APPLICATION_CONTEXT ( 'automotive_design' ) ;
#17429 = VERTEX_POINT ( 'NONE', #16125 ) ;
#17430 = CLOSED_SHELL ( 'NONE', ( #14427, #9550, #7009, #1130, #11581, #2341, #12839, #5361, #16794, #1725, #6753, #2288, #1283, #5749, #13507, #1728, #17289, #9406, #3180, #8700, #2170, #14616, #13964, #1304, #7111, #9840, #13310, #1375, #7793, #1505, #7682, #16921, #16928, #15297, #12818, #14097, #11635, #16107, #8927, #9754, #2962, #4086, #15692, #16347, #20, #19, #1394, #11127, #12598, #14523, #340, #3493, #5639, #7439, #3116, #9476, #17505, #2382, #13509, #14536, #17034, #5595, #9828, #8812, #566, #7350, #16640, #17591, #2634, #13572, #9290, #1437, #13433, #7228, #12607, #11483, #12360, #14310, #6410, #9504, #12249, #15, #15565, #1249, #17255, #15956, #12381, #16019, #6382, #1256, #11082, #11531, #2551, #14985, #5912, #8723, #12622, #2773, #11338 ) ) ;
#17431 = LINE ( 'NONE', #4434, #7316 ) ;
#17432 = DIRECTION ( 'NONE',  ( -1.156482317317869999E-16, 0.000000000000000000, -1.000000000000000000 ) ) ;
#17433 = CARTESIAN_POINT ( 'NONE',  ( -57.08002265617300708, 84.22855780814606419, -124.8487082408420861 ) ) ;
#17434 = ORIENTED_EDGE ( 'NONE', *, *, #116, .T. ) ;
#17435 = DIRECTION ( 'NONE',  ( 0.3420201433256737644, -0.9396926207859066515, 0.000000000000000000 ) ) ;
#17436 = CIRCLE ( 'NONE', #15358, 3.999999999999989786 ) ;
#17438 = VECTOR ( 'NONE', #5643, 1000.000000000000000 ) ;
#17437 = DIRECTION ( 'NONE',  ( 1.000000000000000000, 0.000000000000000000, 0.000000000000000000 ) ) ;
#17439 = DIRECTION ( 'NONE',  ( -0.9396926207859097602, 0.3420201433256649381, -4.890320548438455808E-16 ) ) ;
#17440 = DIRECTION ( 'NONE',  ( -1.000000000000000000, -0.000000000000000000, -0.000000000000000000 ) ) ;
#17441 = EDGE_LOOP ( 'NONE', ( #6676, #17529, #14, #12990 ) ) ;
#17442 = DIRECTION ( 'NONE',  ( 0.000000000000000000, 0.000000000000000000, -1.000000000000000000 ) ) ;
#17443 = DIRECTION ( 'NONE',  ( 1.000000000000000000, 2.062304371594500494E-16, -2.775557561562890858E-16 ) ) ;
#17444 = FACE_OUTER_BOUND ( 'NONE', #2226, .T. ) ;
#17446 = ORIENTED_EDGE ( 'NONE', *, *, #9244, .T. ) ;
#17445 = EDGE_CURVE ( 'NONE', #9165, #14123, #3054, .T. ) ;
#17447 =( GEOMETRIC_REPRESENTATION_CONTEXT ( 3 ) GLOBAL_UNCERTAINTY_ASSIGNED_CONTEXT ( ( #13391 ) ) GLOBAL_UNIT_ASSIGNED_CONTEXT ( ( #9956, #15277, #15473 ) ) REPRESENTATION_CONTEXT ( 'NONE', 'WORKASPACE' ) );
#17448 = DIRECTION ( 'NONE',  ( 0.000000000000000000, 0.000000000000000000, -1.000000000000000000 ) ) ;
#17449 = VECTOR ( 'NONE', #825, 1000.000000000000000 ) ;
#17450 = LINE ( 'NONE', #4542, #3259 ) ;
#17451 = VECTOR ( 'NONE', #8180, 1000.000000000000000 ) ;
#17452 = ORIENTED_EDGE ( 'NONE', *, *, #331, .F. ) ;
#17453 = AXIS2_PLACEMENT_3D ( 'NONE', #4224, #5249, #2832 ) ;
#17454 = ORIENTED_EDGE ( 'NONE', *, *, #11897, .T. ) ;
#17455 = ADVANCED_FACE ( 'NONE', ( #170 ), #8773, .F. ) ;
#17456 = ORIENTED_EDGE ( 'NONE', *, *, #16783, .T. ) ;
#17457 = LINE ( 'NONE', #14913, #3099 ) ;
#17458 = VECTOR ( 'NONE', #1791, 1000.000000000000000 ) ;
#17459 = ORIENTED_EDGE ( 'NONE', *, *, #17850, .F. ) ;
#17460 = DIRECTION ( 'NONE',  ( 0.000000000000000000, 0.000000000000000000, 1.000000000000000000 ) ) ;
#17461 = CARTESIAN_POINT ( 'NONE',  ( -68.94671286412481948, 88.15687341518439268, -15.00000000000001243 ) ) ;
#17462 = CARTESIAN_POINT ( 'NONE',  ( -71.24615306438103346, 43.66964916522919538, -167.1454815528550739 ) ) ;
#17463 = DIRECTION ( 'NONE',  ( -5.204170427930409450E-16, 0.000000000000000000, 1.000000000000000000 ) ) ;
#17464 = ORIENTED_EDGE ( 'NONE', *, *, #15703, .T. ) ;
#17465 = CIRCLE ( 'NONE', #3412, 12.50000000000001066 ) ;
#17466 = DIRECTION ( 'NONE',  ( -1.000000000000000000, 0.000000000000000000, 0.000000000000000000 ) ) ;
#17467 = AXIS2_PLACEMENT_3D ( 'NONE', #16833, #6736, #16542 ) ;
#17468 = FACE_OUTER_BOUND ( 'NONE', #15353, .T. ) ;
#17469 = CARTESIAN_POINT ( 'NONE',  ( -46.03642545851250389, 84.22855780814606419, 68.73600986863397111 ) ) ;
#17470 = DIRECTION ( 'NONE',  ( 1.000000000000000000, 0.000000000000000000, 0.000000000000000000 ) ) ;
#17471 = CARTESIAN_POINT ( 'NONE',  ( -36.12567045178374059, 86.17903909013999453, 55.25386615338222640 ) ) ;
#17472 = DIRECTION ( 'NONE',  ( -5.204170427930409450E-16, 0.000000000000000000, 1.000000000000000000 ) ) ;
#17473 = ORIENTED_EDGE ( 'NONE', *, *, #757, .F. ) ;
#17474 = DIRECTION ( 'NONE',  ( 0.000000000000000000, 0.000000000000000000, 1.000000000000000000 ) ) ;
#17475 = CARTESIAN_POINT ( 'NONE',  ( -71.24615306438086293, 88.54081700456373483, 15.00000000000006928 ) ) ;
#17476 = ORIENTED_EDGE ( 'NONE', *, *, #16783, .F. ) ;
#17477 = ORIENTED_EDGE ( 'NONE', *, *, #14970, .T. ) ;
#17478 = EDGE_CURVE ( 'NONE', #7906, #2272, #17532, .T. ) ;
#17479 = CIRCLE ( 'NONE', #3157, 4.600000000000006750 ) ;
#17480 = EDGE_CURVE ( 'NONE', #4782, #10561, #13250, .T. ) ;
#17481 = ORIENTED_EDGE ( 'NONE', *, *, #13282, .F. ) ;
#17482 = DIRECTION ( 'NONE',  ( 1.000000000000000000, 0.000000000000000000, 5.077734830647302671E-16 ) ) ;
#17483 = CARTESIAN_POINT ( 'NONE',  ( -71.24615306438091977, 79.11603905456372843, -15.00000000000001421 ) ) ;
#17484 = FACE_OUTER_BOUND ( 'NONE', #7071, .T. ) ;
#17485 = DIRECTION ( 'NONE',  ( 0.000000000000000000, 0.000000000000000000, 1.000000000000000000 ) ) ;
#17486 = DIRECTION ( 'NONE',  ( 1.000000000000000000, 0.000000000000000000, 1.047634945911799595E-14 ) ) ;
#17487 = EDGE_CURVE ( 'NONE', #9854, #16012, #71, .T. ) ;
#17488 = LINE ( 'NONE', #14776, #9416 ) ;
#17489 = DIRECTION ( 'NONE',  ( 0.000000000000000000, -3.330669073875448914E-16, -1.000000000000000000 ) ) ;
#17490 = ORIENTED_EDGE ( 'NONE', *, *, #10532, .F. ) ;
#17491 = EDGE_CURVE ( 'NONE', #4210, #17364, #14414, .T. ) ;
#17492 = ADVANCED_FACE ( 'NONE', ( #14473 ), #1561, .F. ) ;
#17493 = DIRECTION ( 'NONE',  ( 1.000000000000000000, 0.000000000000000000, 0.000000000000000000 ) ) ;
#17494 = CARTESIAN_POINT ( 'NONE',  ( -71.24615306438074924, 119.9567435045637609, -15.00000000000001421 ) ) ;
#17495 = EDGE_CURVE ( 'NONE', #10265, #11747, #10509, .T. ) ;
#17496 = LINE ( 'NONE', #16173, #14051 ) ;
#17497 = VERTEX_POINT ( 'NONE', #246 ) ;
#17498 = CARTESIAN_POINT ( 'NONE',  ( -70.71978124295696944, -91.08423613455721579, 5.204170427930421283E-15 ) ) ;
#17499 = CARTESIAN_POINT ( 'NONE',  ( -50.81952187608693805, 73.40930968350535579, 15.00000000000006928 ) ) ;
#17500 = ORIENTED_EDGE ( 'NONE', *, *, #15466, .T. ) ;
#17501 = EDGE_CURVE ( 'NONE', #4498, #10224, #12010, .T. ) ;
#17502 = EDGE_CURVE ( 'NONE', #4616, #16069, #8742, .T. ) ;
#17503 = EDGE_CURVE ( 'NONE', #9222, #11275, #16477, .T. ) ;
#17504 = ORIENTED_EDGE ( 'NONE', *, *, #14067, .F. ) ;
#17505 = ADVANCED_FACE ( 'NONE', ( #17444 ), #1826, .T. ) ;
#17506 = CARTESIAN_POINT ( 'NONE',  ( -55.64822083176820655, 96.64628479562776420, -15.00000000000001421 ) ) ;
#17507 = FACE_BOUND ( 'NONE', #7119, .T. ) ;
#17508 = FACE_OUTER_BOUND ( 'NONE', #3415, .T. ) ;
#17509 = ORIENTED_EDGE ( 'NONE', *, *, #17013, .F. ) ;
#17510 = ORIENTED_EDGE ( 'NONE', *, *, #15805, .T. ) ;
#17511 = DIRECTION ( 'NONE',  ( 0.000000000000000000, 0.000000000000000000, 1.000000000000000000 ) ) ;
#17512 = CARTESIAN_POINT ( 'NONE',  ( -66.20428811384469725, 111.5958523346568967, 25.00000000000000711 ) ) ;
#17513 = FACE_OUTER_BOUND ( 'NONE', #9479, .T. ) ;
#17514 = CARTESIAN_POINT ( 'NONE',  ( -44.78895386838529902, 81.95267818613812949, -167.1454815528550739 ) ) ;
#17515 = ORIENTED_EDGE ( 'NONE', *, *, #6396, .F. ) ;
#17516 = EDGE_CURVE ( 'NONE', #15187, #17628, #6587, .T. ) ;
#17517 = EDGE_CURVE ( 'NONE', #15284, #4575, #2756, .T. ) ;
#17518 = DIRECTION ( 'NONE',  ( -5.204170427930409450E-16, 0.000000000000000000, 1.000000000000000000 ) ) ;
#17519 = ORIENTED_EDGE ( 'NONE', *, *, #803, .T. ) ;
#17520 = CYLINDRICAL_SURFACE ( 'NONE', #11605, 7.500000000000000000 ) ;
#17521 = VERTEX_POINT ( 'NONE', #18004 ) ;
#17522 = ORIENTED_EDGE ( 'NONE', *, *, #6295, .T. ) ;
#17523 = PLANE ( 'NONE',  #3394 ) ;
#17524 = LINE ( 'NONE', #6108, #17133 ) ;
#17525 = ORIENTED_EDGE ( 'NONE', *, *, #5699, .T. ) ;
#17526 = CARTESIAN_POINT ( 'NONE',  ( -71.24615306438109030, 24.82009326522924297, -167.1454815528550739 ) ) ;
#17527 = CARTESIAN_POINT ( 'NONE',  ( -57.08002265617300708, 84.22855780814606419, -28.00000000000000355 ) ) ;
#17528 = PLANE ( 'NONE',  #10899 ) ;
#17529 = ORIENTED_EDGE ( 'NONE', *, *, #4449, .T. ) ;
#17530 = DIRECTION ( 'NONE',  ( -5.204170427930409450E-16, 0.000000000000000000, 1.000000000000000000 ) ) ;
#17531 = DIRECTION ( 'NONE',  ( 1.000000000000000000, 0.000000000000000000, 0.000000000000000000 ) ) ;
#17532 = LINE ( 'NONE', #2966, #17383 ) ;
#17533 = ORIENTED_EDGE ( 'NONE', *, *, #17022, .T. ) ;
#17534 = CARTESIAN_POINT ( 'NONE',  ( -92.59262256747319952, 61.64996188551983636, -25.00000000000000000 ) ) ;
#17535 = CARTESIAN_POINT ( 'NONE',  ( -46.83322972390671879, 84.01587117655466841, -167.1454815528550739 ) ) ;
#17536 = ORIENTED_EDGE ( 'NONE', *, *, #16889, .F. ) ;
#17537 = ORIENTED_EDGE ( 'NONE', *, *, #1627, .F. ) ;
#17538 = ORIENTED_EDGE ( 'NONE', *, *, #14739, .T. ) ;
#17540 = EDGE_CURVE ( 'NONE', #13143, #6193, #5191, .T. ) ;
#17539 = DIRECTION ( 'NONE',  ( 0.000000000000000000, 0.000000000000000000, -1.000000000000000000 ) ) ;
#17541 = DIRECTION ( 'NONE',  ( 1.000000000000000000, 0.000000000000000000, 0.000000000000000000 ) ) ;
#17542 = DIRECTION ( 'NONE',  ( 1.000000000000000000, 0.000000000000000000, 0.000000000000000000 ) ) ;
#17543 = FACE_OUTER_BOUND ( 'NONE', #11387, .T. ) ;
#17544 = FACE_OUTER_BOUND ( 'NONE', #14628, .T. ) ;
#17545 = ORIENTED_EDGE ( 'NONE', *, *, #13183, .T. ) ;
#17546 = PLANE ( 'NONE',  #11664 ) ;
#17547 = DIRECTION ( 'NONE',  ( 1.000000000000000000, 0.000000000000000000, 0.000000000000000000 ) ) ;
#17548 = DIRECTION ( 'NONE',  ( -1.000000000000000000, 0.000000000000000000, 0.000000000000000000 ) ) ;
#17549 = CARTESIAN_POINT ( 'NONE',  ( -68.99615306438120399, -1.746436818337276931, -167.1454815528550739 ) ) ;
#17550 = VECTOR ( 'NONE', #10609, 1000.000000000000000 ) ;
#17551 = CARTESIAN_POINT ( 'NONE',  ( -36.89658380969908791, 90.19024662095814904, 67.07644706209384822 ) ) ;
#17552 = ORIENTED_EDGE ( 'NONE', *, *, #10078, .T. ) ;
#17553 = SHAPE_REPRESENTATION ( 'C-Frame Forged Steel Casing', ( #16217 ), #2819 ) ;
#17554 = VECTOR ( 'NONE', #4871, 1000.000000000000000 ) ;
#17555 = DIRECTION ( 'NONE',  ( 1.000000000000000000, 0.000000000000000000, 0.000000000000000000 ) ) ;
#17556 = VERTEX_POINT ( 'NONE', #7712 ) ;
#17557 = FACE_OUTER_BOUND ( 'NONE', #10244, .T. ) ;
#17558 = LINE ( 'NONE', #6140, #18253 ) ;
#17559 = ORIENTED_EDGE ( 'NONE', *, *, #10743, .T. ) ;
#17560 = ORIENTED_EDGE ( 'NONE', *, *, #10988, .F. ) ;
#17561 = AXIS2_PLACEMENT_3D ( 'NONE', #15446, #11151, #9747 ) ;
#17562 = ORIENTED_EDGE ( 'NONE', *, *, #1138, .F. ) ;
#17563 = DIRECTION ( 'NONE',  ( 1.000000000000000000, 0.000000000000000000, 0.000000000000000000 ) ) ;
#17564 = CARTESIAN_POINT ( 'NONE',  ( 103.5381772159376084, -111.0842361345572158, -57.00000000000000000 ) ) ;
#17565 = CARTESIAN_POINT ( 'NONE',  ( -77.98461495213935279, 81.80210967128928701, 69.60095798084290664 ) ) ;
#17566 = PLANE ( 'NONE',  #15418 ) ;
#17567 = CARTESIAN_POINT ( 'NONE',  ( -68.99615306438080609, 105.0677132816627051, -167.1454815528550739 ) ) ;
#17568 = DIRECTION ( 'NONE',  ( 0.000000000000000000, 0.000000000000000000, 1.000000000000000000 ) ) ;
#17569 = DIRECTION ( 'NONE',  ( 0.000000000000000000, 0.000000000000000000, 1.000000000000000000 ) ) ;
#17570 = EDGE_LOOP ( 'NONE', ( #895, #6544, #10333, #127 ) ) ;
#17571 = DIRECTION ( 'NONE',  ( 2.775557561562890858E-16, 0.000000000000000000, 1.000000000000000000 ) ) ;
#17572 = ADVANCED_FACE ( 'NONE', ( #10707 ), #4908, .T. ) ;
#17573 = FACE_OUTER_BOUND ( 'NONE', #5407, .T. ) ;
#17574 = DIRECTION ( 'NONE',  ( 0.000000000000000000, 0.000000000000000000, 1.000000000000000000 ) ) ;
#17575 = CIRCLE ( 'NONE', #11901, 10.24899999999998812 ) ;
#17576 = ORIENTED_EDGE ( 'NONE', *, *, #14960, .F. ) ;
#17577 = DIRECTION ( 'NONE',  ( 0.000000000000000000, 0.000000000000000000, 1.000000000000000000 ) ) ;
#17578 = CARTESIAN_POINT ( 'NONE',  ( 15.23320273812467462, -111.0842361345572158, 57.00000000000000000 ) ) ;
#17579 = ORIENTED_EDGE ( 'NONE', *, *, #9516, .T. ) ;
#17580 = EDGE_CURVE ( 'NONE', #11429, #6748, #13975, .T. ) ;
#17581 = ORIENTED_EDGE ( 'NONE', *, *, #12899, .T. ) ;
#17582 = EDGE_CURVE ( 'NONE', #11731, #3038, #6398, .T. ) ;
#17583 = DIRECTION ( 'NONE',  ( -5.204170427930409450E-16, 0.000000000000000000, 1.000000000000000000 ) ) ;
#17584 = AXIS2_PLACEMENT_3D ( 'NONE', #14589, #13715, #472 ) ;
#17585 = CYLINDRICAL_SURFACE ( 'NONE', #8515, 3.999999999999996447 ) ;
#17586 = CARTESIAN_POINT ( 'NONE',  ( -68.99615306438066398, 133.9569029881302527, 15.00000000000006928 ) ) ;
#17587 = ORIENTED_EDGE ( 'NONE', *, *, #13922, .F. ) ;
#17588 = VECTOR ( 'NONE', #1105, 1000.000000000000114 ) ;
#17589 = CARTESIAN_POINT ( 'NONE',  ( -68.99615306438086293, 89.97460588813027016, -167.1454815528550739 ) ) ;
#17590 = ORIENTED_EDGE ( 'NONE', *, *, #14327, .F. ) ;
#17591 = ADVANCED_FACE ( 'NONE', ( #12208 ), #9411, .T. ) ;
#17592 = FACE_OUTER_BOUND ( 'NONE', #787, .T. ) ;
#17593 = CARTESIAN_POINT ( 'NONE',  ( -68.99615306438117557, 5.151604338130305827, -167.1454815528550739 ) ) ;
#17594 = CARTESIAN_POINT ( 'NONE',  ( -77.35352728739614747, 89.88064937530401721, 57.54580211461716743 ) ) ;
#17595 = EDGE_CURVE ( 'NONE', #5776, #70, #17979, .T. ) ;
#17596 = FACE_OUTER_BOUND ( 'NONE', #10302, .T. ) ;
#17597 = EDGE_CURVE ( 'NONE', #7613, #6728, #7812, .T. ) ;
#17598 = EDGE_LOOP ( 'NONE', ( #15096, #953, #4555, #10021 ) ) ;
#17599 = CARTESIAN_POINT ( 'NONE',  ( -57.08002265617300708, 84.22855780814606419, -61.50000000000001421 ) ) ;
#17600 = ORIENTED_EDGE ( 'NONE', *, *, #12238, .F. ) ;
#17601 = CYLINDRICAL_SURFACE ( 'NONE', #849, 4.600000000000013856 ) ;
#17602 = ORIENTED_EDGE ( 'NONE', *, *, #4335, .F. ) ;
#17603 = AXIS2_PLACEMENT_3D ( 'NONE', #18198, #9689, #6690 ) ;
#17604 = ADVANCED_FACE ( 'NONE', ( #3590, #3408, #4993 ), #12125, .F. ) ;
#17605 = ORIENTED_EDGE ( 'NONE', *, *, #6889, .F. ) ;
#17606 = VECTOR ( 'NONE', #1003, 1000.000000000000000 ) ;
#17607 = EDGE_LOOP ( 'NONE', ( #7222, #15717, #5596, #3945 ) ) ;
#17608 = EDGE_CURVE ( 'NONE', #6267, #7322, #9216, .T. ) ;
#17609 = PLANE ( 'NONE',  #13889 ) ;
#17610 = EDGE_CURVE ( 'NONE', #11065, #12783, #1865, .T. ) ;
#17611 = DIRECTION ( 'NONE',  ( 0.000000000000000000, 1.000000000000000000, -0.000000000000000000 ) ) ;
#17612 = ORIENTED_EDGE ( 'NONE', *, *, #5852, .T. ) ;
#17613 = DIRECTION ( 'NONE',  ( 0.000000000000000000, 0.000000000000000000, 1.000000000000000000 ) ) ;
#17614 = AXIS2_PLACEMENT_3D ( 'NONE', #2740, #4328, #1521 ) ;
#17615 = DIRECTION ( 'NONE',  ( 1.000000000000000000, 0.000000000000000000, 0.000000000000000000 ) ) ;
#17616 = ORIENTED_EDGE ( 'NONE', *, *, #3091, .T. ) ;
#17617 = ADVANCED_FACE ( 'NONE', ( #17813 ), #16400, .F. ) ;
#17618 = CARTESIAN_POINT ( 'NONE',  ( -57.08002265617300708, 84.22855780814606419, 15.00000000000006928 ) ) ;
#17619 = AXIS2_PLACEMENT_3D ( 'NONE', #12454, #14311, #8421 ) ;
#17620 = VERTEX_POINT ( 'NONE', #2285 ) ;
#17621 = AXIS2_PLACEMENT_3D ( 'NONE', #1956, #1763, #11866 ) ;
#17622 = DIRECTION ( 'NONE',  ( 1.000000000000000000, 0.000000000000000000, 0.000000000000000000 ) ) ;
#17623 = DIRECTION ( 'NONE',  ( 1.000000000000000000, 0.000000000000000000, 5.551115123125786646E-16 ) ) ;
#17624 = ORIENTED_EDGE ( 'NONE', *, *, #16899, .F. ) ;
#17625 = DIRECTION ( 'NONE',  ( -5.204170427930409450E-16, 0.000000000000000000, 1.000000000000000000 ) ) ;
#17626 = COLOUR_RGB ( '',0.7921568627450980005, 0.8196078431372548767, 0.9333333333333333481 ) ;
#17627 = PLANE ( 'NONE',  #1484 ) ;
#17628 = VERTEX_POINT ( 'NONE', #13703 ) ;
#17629 = CIRCLE ( 'NONE', #16725, 10.65431531532567888 ) ;
#17630 = ORIENTED_EDGE ( 'NONE', *, *, #15581, .F. ) ;
#17631 = VECTOR ( 'NONE', #12434, 1000.000000000000000 ) ;
#17632 = VECTOR ( 'NONE', #8675, 1000.000000000000000 ) ;
#17633 = ORIENTED_EDGE ( 'NONE', *, *, #6273, .T. ) ;
#17634 = DIRECTION ( 'NONE',  ( 0.000000000000000000, -5.551115123125748189E-17, -1.000000000000000000 ) ) ;
#17635 = DIRECTION ( 'NONE',  ( -1.000000000000000000, -2.062304371594500740E-16, -0.000000000000000000 ) ) ;
#17636 = ORIENTED_EDGE ( 'NONE', *, *, #3554, .F. ) ;
#17637 = APPLICATION_PROTOCOL_DEFINITION ( 'draft international standard', 'automotive_design', 1998, #17202 ) ;
#17638 = PLANE ( 'NONE',  #7326 ) ;
#17639 = DIRECTION ( 'NONE',  ( 1.000000000000000000, 0.000000000000000000, 0.000000000000000000 ) ) ;
#17640 = DIRECTION ( 'NONE',  ( 0.000000000000000000, 0.000000000000000000, -1.000000000000000000 ) ) ;
#17641 = ORIENTED_EDGE ( 'NONE', *, *, #8896, .T. ) ;
#17642 = CARTESIAN_POINT ( 'NONE',  ( -60.06546592763099568, -91.08423613455721579, -28.18308811886527110 ) ) ;
#17643 = DIRECTION ( 'NONE',  ( 4.124608743189000987E-16, -1.000000000000000000, 0.000000000000000000 ) ) ;
#17644 = CARTESIAN_POINT ( 'NONE',  ( -68.99615306438104767, 27.14275288813030329, -15.00000000000001421 ) ) ;
#17645 = DIRECTION ( 'NONE',  ( 0.000000000000000000, 0.000000000000000000, 1.000000000000000000 ) ) ;
#17646 = CARTESIAN_POINT ( 'NONE',  ( -36.37372457221012922, 88.00379445693184266, 68.99882519264671998 ) ) ;
#17647 = ORIENTED_EDGE ( 'NONE', *, *, #17820, .F. ) ;
#17648 = CIRCLE ( 'NONE', #11101, 180.8515291679561585 ) ;
#17649 = VECTOR ( 'NONE', #165, 1000.000000000000000 ) ;
#17650 = CARTESIAN_POINT ( 'NONE',  ( -60.31105839772099841, 93.95493478196522119, -15.00000000000001421 ) ) ;
#17651 = DIRECTION ( 'NONE',  ( 0.000000000000000000, 0.000000000000000000, 1.000000000000000000 ) ) ;
#17652 = ORIENTED_EDGE ( 'NONE', *, *, #13629, .F. ) ;
#17653 = DIRECTION ( 'NONE',  ( -5.204170427930409450E-16, 0.000000000000000000, 1.000000000000000000 ) ) ;
#17654 = LINE ( 'NONE', #4841, #3903 ) ;
#17655 = ORIENTED_EDGE ( 'NONE', *, *, #12014, .T. ) ;
#17656 = EDGE_LOOP ( 'NONE', ( #8456, #11546, #7371, #4176 ) ) ;
#17657 = AXIS2_PLACEMENT_3D ( 'NONE', #4774, #10875, #12478 ) ;
#17658 = DIRECTION ( 'NONE',  ( -1.000000000000000000, 0.000000000000000000, 0.000000000000000000 ) ) ;
#17659 = ORIENTED_EDGE ( 'NONE', *, *, #18190, .F. ) ;
#17660 = AXIS2_PLACEMENT_3D ( 'NONE', #11995, #680, #7507 ) ;
#17661 = CIRCLE ( 'NONE', #13195, 17.12963335357822814 ) ;
#17662 = DIRECTION ( 'NONE',  ( 1.000000000000000000, 0.000000000000000000, 5.551115123125780730E-16 ) ) ;
#17663 = DIRECTION ( 'NONE',  ( 0.000000000000000000, 0.000000000000000000, -1.000000000000000000 ) ) ;
#17664 = CARTESIAN_POINT ( 'NONE',  ( -71.49209981491081578, 109.8200333694789776, 22.42650986270964353 ) ) ;
#17665 = DIRECTION ( 'NONE',  ( 4.029365176583844474E-15, 0.000000000000000000, -1.000000000000000000 ) ) ;
#17666 = CARTESIAN_POINT ( 'NONE',  ( -71.24615306438079188, 101.1071876045637339, 15.00000000000006928 ) ) ;
#17667 = DIRECTION ( 'NONE',  ( -1.000000000000000000, 0.000000000000000000, -0.000000000000000000 ) ) ;
#17668 = ORIENTED_EDGE ( 'NONE', *, *, #1081, .F. ) ;
#17669 = CARTESIAN_POINT ( 'NONE',  ( 105.4583593777967963, -32.62665103886256190, 7.000000000000010658 ) ) ;
#17670 = CARTESIAN_POINT ( 'NONE',  ( -7.840676406241780860, 112.6569076202650308, 97.49999999999998579 ) ) ;
#17671 = DIRECTION ( 'NONE',  ( 1.000000000000000000, 0.000000000000000000, 0.000000000000000000 ) ) ;
#17672 = ORIENTED_EDGE ( 'NONE', *, *, #10752, .T. ) ;
#17673 = AXIS2_PLACEMENT_3D ( 'NONE', #3503, #17900, #17623 ) ;
#17674 = DIRECTION ( 'NONE',  ( 0.000000000000000000, 0.000000000000000000, 1.000000000000000000 ) ) ;
#17675 = VECTOR ( 'NONE', #5693, 1000.000000000000000 ) ;
#17676 = CARTESIAN_POINT ( 'NONE',  ( -71.24615306438106188, 37.38646386522923137, 15.00000000000006928 ) ) ;
#17677 = ORIENTED_EDGE ( 'NONE', *, *, #11107, .T. ) ;
#17678 = EDGE_LOOP ( 'NONE', ( #16174, #13365, #15265, #9572 ) ) ;
#17679 = PRODUCT_DEFINITION_CONTEXT ( 'detailed design', #17428, 'design' ) ;
#17680 = VECTOR ( 'NONE', #5905, 1000.000000000000000 ) ;
#17681 = EDGE_CURVE ( 'NONE', #10723, #7354, #5753, .T. ) ;
#17682 = CARTESIAN_POINT ( 'NONE',  ( -68.99615306438100504, 39.09426763166271002, -167.1454815528550739 ) ) ;
#17683 = DIRECTION ( 'NONE',  ( 0.9396926207859145341, 0.3420201433256518375, 0.000000000000000000 ) ) ;
#17684 = CARTESIAN_POINT ( 'NONE',  ( -71.24615306438103346, 47.70011255456374499, -167.1454815528550739 ) ) ;
#17685 = LINE ( 'NONE', #4967, #686 ) ;
#17686 = EDGE_LOOP ( 'NONE', ( #5592, #5079 ) ) ;
#17687 = AXIS2_PLACEMENT_3D ( 'NONE', #9309, #15004, #799 ) ;
#17688 = LINE ( 'NONE', #6265, #6859 ) ;
#17689 = AXIS2_PLACEMENT_3D ( 'NONE', #8447, #8265, #9765 ) ;
#17690 = CARTESIAN_POINT ( 'NONE',  ( -57.08002265617300708, 84.22855780814606419, -62.50000000000000000 ) ) ;
#17691 = ORIENTED_EDGE ( 'NONE', *, *, #12712, .T. ) ;
#17692 = DIRECTION ( 'NONE',  ( 6.950654929607131638E-15, 0.000000000000000000, -1.000000000000000000 ) ) ;
#17693 = LINE ( 'NONE', #10778, #3041 ) ;
#17694 = CARTESIAN_POINT ( 'NONE',  ( -68.99615306438089135, 67.98345733813025049, -15.00000000000001421 ) ) ;
#17695 = LINE ( 'NONE', #9199, #675 ) ;
#17696 = ORIENTED_EDGE ( 'NONE', *, *, #4083, .T. ) ;
#17697 = EDGE_CURVE ( 'NONE', #9204, #5292, #7843, .T. ) ;
#17698 = CARTESIAN_POINT ( 'NONE',  ( -68.99615306438084872, 89.97460588813027016, -15.00000000000001421 ) ) ;
#17699 = EDGE_LOOP ( 'NONE', ( #220, #8433, #2568, #15248 ) ) ;
#17700 = CIRCLE ( 'NONE', #12955, 4.025000000000000355 ) ;
#17701 = ADVANCED_FACE ( 'NONE', ( #9585 ), #12507, .T. ) ;
#17702 = CARTESIAN_POINT ( 'NONE',  ( -27.71117476891160081, 84.22855780814606419, -28.00000000000000355 ) ) ;
#17703 = EDGE_LOOP ( 'NONE', ( #4889, #3587, #16388, #7388 ) ) ;
#17704 = VECTOR ( 'NONE', #9252, 1000.000000000000000 ) ;
#17705 = AXIS2_PLACEMENT_3D ( 'NONE', #14158, #9847, #3950 ) ;
#17706 = VECTOR ( 'NONE', #15719, 1000.000000000000000 ) ;
#17707 = VERTEX_POINT ( 'NONE', #988 ) ;
#17708 = EDGE_CURVE ( 'NONE', #10347, #9500, #17399, .T. ) ;
#17709 = EDGE_CURVE ( 'NONE', #4616, #5567, #2767, .T. ) ;
#17710 = PLANE ( 'NONE',  #12704 ) ;
#17711 = CARTESIAN_POINT ( 'NONE',  ( -97.59262256747321373, 110.5691553257988460, -26.35917033480641436 ) ) ;
#17712 = VECTOR ( 'NONE', #7726, 1000.000000000000000 ) ;
#17713 = VERTEX_POINT ( 'NONE', #18112 ) ;
#17714 = EDGE_CURVE ( 'NONE', #8377, #4219, #11446, .T. ) ;
#17715 = DIRECTION ( 'NONE',  ( -0.7071067811864494290, 0.000000000000000000, 0.7071067811866454944 ) ) ;
#17716 = DIRECTION ( 'NONE',  ( 1.000000000000000000, 2.062304371594500494E-16, -0.000000000000000000 ) ) ;
#17717 = ORIENTED_EDGE ( 'NONE', *, *, #8591, .F. ) ;
#17718 = CARTESIAN_POINT ( 'NONE',  ( -97.59262256747319952, 110.5691553257988460, 22.35917033480641791 ) ) ;
#17719 = EDGE_CURVE ( 'NONE', #17860, #14842, #9690, .T. ) ;
#17720 = CIRCLE ( 'NONE', #18353, 4.000000000000024869 ) ;
#17721 = ORIENTED_EDGE ( 'NONE', *, *, #3956, .T. ) ;
#17722 = CIRCLE ( 'NONE', #412, 18.23991632971911514 ) ;
#17723 = EDGE_CURVE ( 'NONE', #7906, #1253, #8288, .T. ) ;
#17724 = LINE ( 'NONE', #427, #17090 ) ;
#17725 = CARTESIAN_POINT ( 'NONE',  ( -67.42362413453201953, 107.1062079628228503, 25.00000000000000000 ) ) ;
#17726 = EDGE_CURVE ( 'NONE', #11067, #15472, #16780, .T. ) ;
#17727 = CARTESIAN_POINT ( 'NONE',  ( -71.24615306438106188, 38.27533460456375281, -15.00000000000001421 ) ) ;
#17728 = EDGE_CURVE ( 'NONE', #16781, #3544, #16975, .T. ) ;
#17729 = CLOSED_SHELL ( 'NONE', ( #1778, #690, #5036, #12490, #1528, #15240, #8823, #1055, #10262, #11865, #10873, #1855, #6817, #17617, #18064, #18445, #2882, #5086, #16434, #14737, #6523, #5670, #7657, #12251, #6756, #10696, #5597, #5498, #10318, #6182, #5478, #16459, #15563, #373, #215, #16828 ) ) ;
#17730 = CARTESIAN_POINT ( 'NONE',  ( -77.14491745292022529, -93.39009998357853704, -44.16867553823941961 ) ) ;
#17731 = VERTEX_POINT ( 'NONE', #16682 ) ;
#17732 = ORIENTED_EDGE ( 'NONE', *, *, #13474, .F. ) ;
#17733 = EDGE_CURVE ( 'NONE', #5564, #17891, #6643, .T. ) ;
#17734 = EDGE_CURVE ( 'NONE', #18456, #14915, #2480, .T. ) ;
#17735 = AXIS2_PLACEMENT_3D ( 'NONE', #17184, #15775, #3993 ) ;
#17736 = CIRCLE ( 'NONE', #3401, 10.24900000000000055 ) ;
#17737 = PRODUCT_DEFINITION_SHAPE ( 'NONE', 'NONE',  #18531 ) ;
#17738 = ORIENTED_EDGE ( 'NONE', *, *, #5739, .T. ) ;
#17739 = LINE ( 'NONE', #893, #12376 ) ;
#17740 = DIRECTION ( 'NONE',  ( 0.000000000000000000, 0.000000000000000000, -1.000000000000000000 ) ) ;
#17741 = ORIENTED_EDGE ( 'NONE', *, *, #716, .T. ) ;
#17742 = DIRECTION ( 'NONE',  ( 0.000000000000000000, 0.000000000000000000, 1.000000000000000000 ) ) ;
#17743 = LINE ( 'NONE', #4925, #9666 ) ;
#17744 = DIRECTION ( 'NONE',  ( 1.156482317317869999E-16, 0.000000000000000000, 1.000000000000000000 ) ) ;
#17745 = ORIENTED_EDGE ( 'NONE', *, *, #11565, .F. ) ;
#17746 = LINE ( 'NONE', #13354, #6583 ) ;
#17747 = DIRECTION ( 'NONE',  ( 1.000000000000000000, 0.000000000000000000, 0.000000000000000000 ) ) ;
#17748 = DIRECTION ( 'NONE',  ( 1.156482317317869999E-16, 0.000000000000000000, 1.000000000000000000 ) ) ;
#17749 = CARTESIAN_POINT ( 'NONE',  ( -9.409811683556181805, 39.33212575317277526, 34.01304937313500432 ) ) ;
#17750 = ORIENTED_EDGE ( 'NONE', *, *, #17714, .T. ) ;
#17751 = VECTOR ( 'NONE', #4268, 1000.000000000000000 ) ;
#17752 = CIRCLE ( 'NONE', #13883, 4.962965561209093046 ) ;
#17753 = VECTOR ( 'NONE', #13697, 1000.000000000000000 ) ;
#17754 = VECTOR ( 'NONE', #7217, 1000.000000000000000 ) ;
#17755 = LINE ( 'NONE', #13549, #9399 ) ;
#17756 = CARTESIAN_POINT ( 'NONE',  ( -46.89970808030100358, 83.04399200740388665, -167.1454815528550739 ) ) ;
#17757 = EDGE_CURVE ( 'NONE', #12828, #5881, #1273, .T. ) ;
#17758 = ORIENTED_EDGE ( 'NONE', *, *, #6856, .T. ) ;
#17759 = DIRECTION ( 'NONE',  ( 0.000000000000000000, 0.000000000000000000, 1.000000000000000000 ) ) ;
#17760 = CARTESIAN_POINT ( 'NONE',  ( -123.4618227840623632, -111.0842361345572158, 57.00000000000000000 ) ) ;
#17761 = ORIENTED_EDGE ( 'NONE', *, *, #6767, .F. ) ;
#17762 = VERTEX_POINT ( 'NONE', #11194 ) ;
#17763 = VECTOR ( 'NONE', #3774, 1000.000000000000000 ) ;
#17764 = DIRECTION ( 'NONE',  ( -1.000000000000000000, 0.000000000000000000, 0.000000000000000000 ) ) ;
#17765 = EDGE_LOOP ( 'NONE', ( #7075, #6300, #9297, #9296 ) ) ;
#17766 = CIRCLE ( 'NONE', #11223, 17.12963335357822814 ) ;
#17767 = CARTESIAN_POINT ( 'NONE',  ( -71.24615306438070661, 187.7866419848965052, -15.00000000000001421 ) ) ;
#17768 = FACE_OUTER_BOUND ( 'NONE', #2133, .T. ) ;
#17769 = LINE ( 'NONE', #1967, #16251 ) ;
#17770 = DIRECTION ( 'NONE',  ( 0.9396926207859084279, 0.3420201433256686574, 0.000000000000000000 ) ) ;
#17771 = LINE ( 'NONE', #9256, #4342 ) ;
#17772 = CARTESIAN_POINT ( 'NONE',  ( 0.000000000000000000, 0.000000000000000000, -57.00000000000000000 ) ) ;
#17773 = EDGE_LOOP ( 'NONE', ( #8964, #545, #1078, #16737 ) ) ;
#17774 = CARTESIAN_POINT ( 'NONE',  ( -75.66356596311996441, 61.48658486655093469, -24.60062213568815537 ) ) ;
#17775 = CARTESIAN_POINT ( 'NONE',  ( -71.24615306438060713, 145.0894847045638016, 15.00000000000006928 ) ) ;
#17776 = ORIENTED_EDGE ( 'NONE', *, *, #13630, .F. ) ;
#17777 = AXIS2_PLACEMENT_3D ( 'NONE', #11046, #945, #12367 ) ;
#17778 = LINE ( 'NONE', #17861, #6421 ) ;
#17779 = DIRECTION ( 'NONE',  ( 0.000000000000000000, 0.000000000000000000, 1.000000000000000000 ) ) ;
#17780 = VERTEX_POINT ( 'NONE', #16886 ) ;
#17781 = EDGE_LOOP ( 'NONE', ( #6189, #12726, #4565, #6827 ) ) ;
#17782 = DIRECTION ( 'NONE',  ( 1.156482317317869999E-16, 0.000000000000000000, 1.000000000000000000 ) ) ;
#17783 = CARTESIAN_POINT ( 'NONE',  ( -92.59262256747318531, 0.3328663868096687350, 25.00000000000000000 ) ) ;
#17784 = CARTESIAN_POINT ( 'NONE',  ( -86.44887054343442401, 84.22855780814606419, -28.00000000000000355 ) ) ;
#17785 = ADVANCED_FACE ( 'NONE', ( #6975 ), #1097, .T. ) ;
#17786 = DIRECTION ( 'NONE',  ( 0.000000000000000000, -5.551115123125747573E-17, -1.000000000000000000 ) ) ;
#17787 = ORIENTED_EDGE ( 'NONE', *, *, #5830, .T. ) ;
#17788 = DIRECTION ( 'NONE',  ( 1.156482317317869999E-16, 0.000000000000000000, 1.000000000000000000 ) ) ;
#17789 = VECTOR ( 'NONE', #18423, 1000.000000000000114 ) ;
#17790 = AXIS2_PLACEMENT_3D ( 'NONE', #498, #7343, #10331 ) ;
#17791 = CARTESIAN_POINT ( 'NONE',  ( 6.212139635163038687E-15, 5.948846446048876579, -2.696295709017856534 ) ) ;
#17792 = ORIENTED_EDGE ( 'NONE', *, *, #8148, .F. ) ;
#17793 = DIRECTION ( 'NONE',  ( 1.000000000000000000, 0.000000000000000000, 6.950654929607132427E-15 ) ) ;
#17794 = CARTESIAN_POINT ( 'NONE',  ( -67.46561775476841660, 81.24207102880470188, -15.00000000000001421 ) ) ;
#17795 = CARTESIAN_POINT ( 'NONE',  ( -78.10200533711912385, 85.21341043856777731, 55.06082720658116614 ) ) ;
#17796 = FACE_OUTER_BOUND ( 'NONE', #3706, .T. ) ;
#17797 = ORIENTED_EDGE ( 'NONE', *, *, #17836, .T. ) ;
#17798 = DIRECTION ( 'NONE',  ( 1.000000000000000000, 2.062304371594500494E-16, 0.000000000000000000 ) ) ;
#17799 = ORIENTED_EDGE ( 'NONE', *, *, #10650, .F. ) ;
#17800 = CARTESIAN_POINT ( 'NONE',  ( -68.99615306438072082, 140.2400882881302948, -167.1454815528550739 ) ) ;
#17801 = ORIENTED_EDGE ( 'NONE', *, *, #10196, .F. ) ;
#17802 = ORIENTED_EDGE ( 'NONE', *, *, #9045, .F. ) ;
#17803 = DIRECTION ( 'NONE',  ( 0.000000000000000000, 0.000000000000000000, -1.000000000000000000 ) ) ;
#17804 = DIRECTION ( 'NONE',  ( 0.000000000000000000, 0.000000000000000000, 1.000000000000000000 ) ) ;
#17805 = ORIENTED_EDGE ( 'NONE', *, *, #15690, .T. ) ;
#17806 = EDGE_CURVE ( 'NONE', #2040, #9854, #11289, .T. ) ;
#17807 = LINE ( 'NONE', #7805, #2728 ) ;
#17808 = CARTESIAN_POINT ( 'NONE',  ( -47.59681378869034774, 80.34130291867735707, 15.00000000000006928 ) ) ;
#17809 = ORIENTED_EDGE ( 'NONE', *, *, #1831, .F. ) ;
#17810 = CARTESIAN_POINT ( 'NONE',  ( -57.89103256796045116, 73.45256821284057480, 15.00000000000006928 ) ) ;
#17811 = ORIENTED_EDGE ( 'NONE', *, *, #9237, .F. ) ;
#17812 = CYLINDRICAL_SURFACE ( 'NONE', #11426, 4.599999999999999645 ) ;
#17813 = FACE_OUTER_BOUND ( 'NONE', #7966, .T. ) ;
#17814 = ORIENTED_EDGE ( 'NONE', *, *, #8486, .F. ) ;
#17815 = ADVANCED_FACE ( 'NONE', ( #5287 ), #9461, .F. ) ;
#17816 = CARTESIAN_POINT ( 'NONE',  ( -68.99615306438094819, 71.12504998813029999, -167.1454815528550739 ) ) ;
#17817 = DIRECTION ( 'NONE',  ( 1.000000000000000000, 1.119176436114069332E-16, 0.000000000000000000 ) ) ;
#17818 = ORIENTED_EDGE ( 'NONE', *, *, #8912, .F. ) ;
#17819 = ORIENTED_EDGE ( 'NONE', *, *, #11548, .F. ) ;
#17820 = EDGE_CURVE ( 'NONE', #15989, #15598, #9641, .T. ) ;
#17821 = EDGE_LOOP ( 'NONE', ( #11574, #11540, #10812, #1380, #13425, #219, #3957, #13986 ) ) ;
#17822 = EDGE_CURVE ( 'NONE', #10461, #17429, #5250, .T. ) ;
#17823 = DIRECTION ( 'NONE',  ( 1.000000000000000000, 0.000000000000000000, 0.000000000000000000 ) ) ;
#17824 = DIRECTION ( 'NONE',  ( 0.000000000000000000, 0.000000000000000000, 1.000000000000000000 ) ) ;
#17825 = EDGE_CURVE ( 'NONE', #6193, #3274, #668, .T. ) ;
#17826 = ORIENTED_EDGE ( 'NONE', *, *, #13813, .T. ) ;
#17827 = DIRECTION ( 'NONE',  ( 0.000000000000000000, 0.000000000000000000, 1.000000000000000000 ) ) ;
#17828 = DIRECTION ( 'NONE',  ( -2.062304371594500494E-16, 1.000000000000000000, -0.000000000000000000 ) ) ;
#17829 = DIRECTION ( 'NONE',  ( 3.223492141267075737E-15, -0.000000000000000000, -1.000000000000000000 ) ) ;
#17830 = EDGE_LOOP ( 'NONE', ( #13364, #13921, #7877, #6124, #830, #12005, #17647, #18432, #17456, #12320, #15329, #7336, #3140, #6201, #14817, #18518, #12534 ) ) ;
#17831 = DIRECTION ( 'NONE',  ( 1.000000000000000000, 0.000000000000000000, 0.000000000000000000 ) ) ;
#17832 = DIRECTION ( 'NONE',  ( -0.000000000000000000, -0.000000000000000000, 1.000000000000000000 ) ) ;
#17833 = CARTESIAN_POINT ( 'NONE',  ( -71.24615306438070661, 137.9174286652292096, -167.1454815528550739 ) ) ;
#17834 = CARTESIAN_POINT ( 'NONE',  ( 4.699999999999995737, 0.000000000000000000, 0.000000000000000000 ) ) ;
#17835 = ORIENTED_EDGE ( 'NONE', *, *, #12951, .T. ) ;
#17836 = EDGE_CURVE ( 'NONE', #17497, #2025, #16464, .T. ) ;
#17837 = ADVANCED_FACE ( 'NONE', ( #13487 ), #2339, .T. ) ;
#17838 = EDGE_CURVE ( 'NONE', #8099, #12661, #10823, .T. ) ;
#17839 = DIRECTION ( 'NONE',  ( -1.000000000000000000, -0.000000000000000000, -0.000000000000000000 ) ) ;
#17840 = DIRECTION ( 'NONE',  ( 0.3420201433256649937, 0.9396926207859097602, -0.000000000000000000 ) ) ;
#17841 = ORIENTED_EDGE ( 'NONE', *, *, #14826, .F. ) ;
#17842 = EDGE_CURVE ( 'NONE', #197, #11711, #8141, .T. ) ;
#17843 = DIRECTION ( 'NONE',  ( -1.000000000000000000, 0.000000000000000000, 0.000000000000000000 ) ) ;
#17844 = CARTESIAN_POINT ( 'NONE',  ( -37.06518108615770046, 77.72307496574234165, 58.73557318418679785 ) ) ;
#17845 = ORIENTED_EDGE ( 'NONE', *, *, #7223, .F. ) ;
#17846 = ORIENTED_EDGE ( 'NONE', *, *, #6061, .T. ) ;
#17847 = ADVANCED_FACE ( 'NONE', ( #8152 ), #18071, .T. ) ;
#17848 = DIRECTION ( 'NONE',  ( 1.000000000000000000, 0.000000000000000000, 0.000000000000000000 ) ) ;
#17849 = VERTEX_POINT ( 'NONE', #6261 ) ;
#17850 = EDGE_CURVE ( 'NONE', #11906, #5703, #4872, .T. ) ;
#17851 = DIRECTION ( 'NONE',  ( -0.000000000000000000, -0.000000000000000000, -1.000000000000000000 ) ) ;
#17852 = CARTESIAN_POINT ( 'NONE',  ( -70.06856178257687873, 57.88796029049330372, 22.35917033480642502 ) ) ;
#17853 = EDGE_CURVE ( 'NONE', #12932, #13576, #7869, .T. ) ;
#17854 = DIRECTION ( 'NONE',  ( -1.000000000000000000, 0.000000000000000000, 0.000000000000000000 ) ) ;
#17855 = DIRECTION ( 'NONE',  ( 1.000000000000000000, 0.000000000000000000, 0.000000000000000000 ) ) ;
#17856 = CARTESIAN_POINT ( 'NONE',  ( -57.08002265617301418, 106.1506877598988154, 92.50000000000000000 ) ) ;
#17857 = ORIENTED_EDGE ( 'NONE', *, *, #1063, .T. ) ;
#17858 = CARTESIAN_POINT ( 'NONE',  ( -72.80844527697490776, 59.42543905650232716, -22.66411427748654361 ) ) ;
#17859 = CARTESIAN_POINT ( 'NONE',  ( -86.44887054343442401, 84.22855780814606419, 25.00000000000000355 ) ) ;
#17860 = VERTEX_POINT ( 'NONE', #3842 ) ;
#17861 = CARTESIAN_POINT ( 'NONE',  ( -71.24615306438070661, 147.3422066152292871, -167.1454815528550739 ) ) ;
#17862 = DIRECTION ( 'NONE',  ( -0.000000000000000000, -0.000000000000000000, -1.000000000000000000 ) ) ;
#17863 = ORIENTED_EDGE ( 'NONE', *, *, #18144, .F. ) ;
#17864 = AXIS2_PLACEMENT_3D ( 'NONE', #1157, #3954, #9667 ) ;
#17865 = ORIENTED_EDGE ( 'NONE', *, *, #2544, .F. ) ;
#17866 = B_SPLINE_CURVE_WITH_KNOTS ( 'NONE', 3,
 ( #9821, #15436, #1217, #16721, #1126, #10016 ),
 .UNSPECIFIED., .F., .F.,
 ( 4, 2, 4 ),
 ( 0.01913986446880888009, 0.02104055318064360774, 0.02294124189247833887 ),
 .UNSPECIFIED. ) ;
#17867 = DIRECTION ( 'NONE',  ( 1.000000000000000000, 0.000000000000000000, 3.771137991253928573E-16 ) ) ;
#17868 = DIRECTION ( 'NONE',  ( 0.000000000000000000, 5.551115123125747573E-17, 1.000000000000000000 ) ) ;
#17869 = CARTESIAN_POINT ( 'NONE',  ( -57.08002265617300708, 84.22855780814606419, -167.1454815528550739 ) ) ;
#17870 = DIRECTION ( 'NONE',  ( 0.000000000000000000, 0.000000000000000000, 1.000000000000000000 ) ) ;
#17871 = VERTEX_POINT ( 'NONE', #9547 ) ;
#17872 = CARTESIAN_POINT ( 'NONE',  ( -71.24615306438117557, 2.828944715229236628, 15.00000000000006928 ) ) ;
#17873 = CARTESIAN_POINT ( 'NONE',  ( 0.01372220897663909388, 5.309964801958091840, -3.802871176606228865 ) ) ;
#17874 = ORIENTED_EDGE ( 'NONE', *, *, #14291, .F. ) ;
#17875 = CIRCLE ( 'NONE', #18184, 22.04359719766050318 ) ;
#17876 = CARTESIAN_POINT ( 'NONE',  ( -71.24615306438086293, 100.2183168652291982, 15.00000000000006928 ) ) ;
#17877 = CARTESIAN_POINT ( 'NONE',  ( -127.5926225674731995, 47.87487112387803023, -15.00000000000000355 ) ) ;
#17878 = CARTESIAN_POINT ( 'NONE',  ( -76.74178926456770000, 91.72841893195355567, 62.99632217189364525 ) ) ;
#17879 = CARTESIAN_POINT ( 'NONE',  ( 0.2565376335216897341, -2.516992571280221913, -6.500000000000063949 ) ) ;
#17880 = EDGE_LOOP ( 'NONE', ( #13323, #2522, #6226, #12766 ) ) ;
#17881 = DIRECTION ( 'NONE',  ( 0.000000000000000000, 0.000000000000000000, 1.000000000000000000 ) ) ;
#17882 = EDGE_LOOP ( 'NONE', ( #8976, #6794, #1503, #6621 ) ) ;
#17883 = LINE ( 'NONE', #13505, #9207 ) ;
#17884 = ORIENTED_EDGE ( 'NONE', *, *, #5020, .T. ) ;
#17885 = PRODUCT ( 'Axle Retaining Ring', 'Axle Retaining Ring', '', ( #15179 ) ) ;
#17886 = EDGE_CURVE ( 'NONE', #1000, #18335, #673, .T. ) ;
#17887 = VERTEX_POINT ( 'NONE', #7776 ) ;
#17888 = EDGE_CURVE ( 'NONE', #12417, #8597, #16370, .T. ) ;
#17889 = CARTESIAN_POINT ( 'NONE',  ( -52.17699016282484337, 93.22868410554724505, -15.00000000000001421 ) ) ;
#17890 = CARTESIAN_POINT ( 'NONE',  ( -57.08002265617300708, 84.22855780814606419, -167.1454815528550739 ) ) ;
#17891 = VERTEX_POINT ( 'NONE', #15068 ) ;
#17892 = DIRECTION ( 'NONE',  ( 0.000000000000000000, 1.000000000000000000, 0.000000000000000000 ) ) ;
#17893 = LINE ( 'NONE', #11185, #17451 ) ;
#17894 = VERTEX_POINT ( 'NONE', #2159 ) ;
#17895 =( NAMED_UNIT ( * ) SI_UNIT ( $, .STERADIAN. ) SOLID_ANGLE_UNIT ( ) );
#17896 = DIRECTION ( 'NONE',  ( 0.000000000000000000, -5.551115123125748189E-17, -1.000000000000000000 ) ) ;
#17897 = ORIENTED_EDGE ( 'NONE', *, *, #699, .F. ) ;
#17898 = VECTOR ( 'NONE', #5760, 1000.000000000000000 ) ;
#17899 = CARTESIAN_POINT ( 'NONE',  ( 276.3098885457529832, -32.62665103886256190, 7.000000000000010658 ) ) ;
#17900 = DIRECTION ( 'NONE',  ( -5.204170427930409450E-16, 0.000000000000000000, 1.000000000000000000 ) ) ;
#17901 = ORIENTED_EDGE ( 'NONE', *, *, #5942, .F. ) ;
#17902 = VECTOR ( 'NONE', #16695, 1000.000000000000000 ) ;
#17903 = DIRECTION ( 'NONE',  ( 1.000000000000000000, 0.000000000000000000, 0.000000000000000000 ) ) ;
#17904 = DIRECTION ( 'NONE',  ( -1.000000000000000000, -0.000000000000000000, -0.000000000000000000 ) ) ;
#17905 = ORIENTED_EDGE ( 'NONE', *, *, #16102, .T. ) ;
#17906 = ORIENTED_EDGE ( 'NONE', *, *, #8390, .T. ) ;
#17907 = AXIS2_PLACEMENT_3D ( 'NONE', #9360, #942, #7858 ) ;
#17908 = CARTESIAN_POINT ( 'NONE',  ( -71.24615306438104767, 22.56737135456382148, 15.00000000000006928 ) ) ;
#17909 = DIRECTION ( 'NONE',  ( 1.000000000000000000, 0.000000000000000000, 0.000000000000000000 ) ) ;
#17910 = EDGE_LOOP ( 'NONE', ( #263, #5205, #9068, #13027, #3315 ) ) ;
#17911 = EDGE_CURVE ( 'NONE', #8947, #10723, #7536, .T. ) ;
#17912 = AXIS2_PLACEMENT_3D ( 'NONE', #3265, #1690, #14512 ) ;
#17913 = CARTESIAN_POINT ( 'NONE',  ( -68.99615306438097662, 61.70027203813028649, 15.00000000000006928 ) ) ;
#17914 = DIRECTION ( 'NONE',  ( 0.000000000000000000, 1.000000000000000000, 0.000000000000000000 ) ) ;
#17915 = AXIS2_PLACEMENT_3D ( 'NONE', #3729, #2313, #9160 ) ;
#17916 = CARTESIAN_POINT ( 'NONE',  ( 1.461703886464493563, 3.647763842320571825, 49.46183131592236037 ) ) ;
#17917 = DIRECTION ( 'NONE',  ( -1.000000000000000000, 2.826528109797569363E-15, 0.000000000000000000 ) ) ;
#17918 = ORIENTED_EDGE ( 'NONE', *, *, #11507, .T. ) ;
#17919 = DIRECTION ( 'NONE',  ( 0.000000000000000000, 1.000000000000000000, 2.775557561562874095E-16 ) ) ;
#17920 = DIRECTION ( 'NONE',  ( 0.000000000000000000, 0.000000000000000000, -1.000000000000000000 ) ) ;
#17921 = DIRECTION ( 'NONE',  ( -0.5150380749100562650, 0.000000000000000000, 0.8571673007021111124 ) ) ;
#17922 = CARTESIAN_POINT ( 'NONE',  ( -57.08002265617300708, 84.22855780814606419, 15.00000000000006928 ) ) ;
#17923 = ORIENTED_EDGE ( 'NONE', *, *, #3655, .F. ) ;
#17924 = CIRCLE ( 'NONE', #4777, 12.49999999999999645 ) ;
#17925 = LINE ( 'NONE', #3523, #12707 ) ;
#17926 = DIRECTION ( 'NONE',  ( -0.000000000000000000, -1.000000000000000000, -0.000000000000000000 ) ) ;
#17928 = EDGE_CURVE ( 'NONE', #14698, #16085, #9945, .T. ) ;
#17927 = CIRCLE ( 'NONE', #7202, 12.50000000000000355 ) ;
#17929 = ORIENTED_EDGE ( 'NONE', *, *, #2974, .T. ) ;
#17930 = DIRECTION ( 'NONE',  ( -1.000000000000000000, 0.000000000000000000, 0.000000000000000000 ) ) ;
#17931 = VECTOR ( 'NONE', #16615, 1000.000000000000000 ) ;
#17932 = CARTESIAN_POINT ( 'NONE',  ( -36.80564135947743409, 78.57985073358729267, 57.54245165641173543 ) ) ;
#17933 = EDGE_LOOP ( 'NONE', ( #17323, #9778 ) ) ;
#17934 = VECTOR ( 'NONE', #1680, 1000.000000000000227 ) ;
#17935 = VERTEX_POINT ( 'NONE', #13673 ) ;
#17936 = CARTESIAN_POINT ( 'NONE',  ( -76.06514409945376087, 73.26749283226919829, 102.5000000000000000 ) ) ;
#17937 = EDGE_CURVE ( 'NONE', #1867, #2089, #8046, .T. ) ;
#17938 = VECTOR ( 'NONE', #6871, 1000.000000000000000 ) ;
#17939 = ORIENTED_EDGE ( 'NONE', *, *, #16007, .F. ) ;
#17940 = EDGE_CURVE ( 'NONE', #6562, #16328, #12275, .T. ) ;
#17941 = DIRECTION ( 'NONE',  ( -0.000000000000000000, 0.000000000000000000, 1.000000000000000000 ) ) ;
#17942 = LINE ( 'NONE', #547, #12668 ) ;
#17943 = DIRECTION ( 'NONE',  ( 0.000000000000000000, 0.000000000000000000, 1.000000000000000000 ) ) ;
#17944 = DIRECTION ( 'NONE',  ( 0.000000000000000000, 0.000000000000000000, 1.000000000000000000 ) ) ;
#17945 = CIRCLE ( 'NONE', #3305, 4.999999999999997335 ) ;
#17946 = VECTOR ( 'NONE', #6682, 1000.000000000000000 ) ;
#17947 = LINE ( 'NONE', #11141, #15978 ) ;
#17948 = CYLINDRICAL_SURFACE ( 'NONE', #5141, 4.599999999999992539 ) ;
#17949 = ORIENTED_EDGE ( 'NONE', *, *, #9255, .F. ) ;
#17950 = EDGE_CURVE ( 'NONE', #6278, #626, #14139, .T. ) ;
#17951 = PLANE ( 'NONE',  #3975 ) ;
#17952 = FACE_OUTER_BOUND ( 'NONE', #6213, .T. ) ;
#17953 = ADVANCED_FACE ( 'NONE', ( #4051 ), #14431, .F. ) ;
#17954 = ORIENTED_EDGE ( 'NONE', *, *, #13378, .F. ) ;
#17955 = VECTOR ( 'NONE', #10474, 999.9999999999998863 ) ;
#17956 = CARTESIAN_POINT ( 'NONE',  ( -78.12361985383350316, 84.22855780814606419, 55.00000000000001421 ) ) ;
#17957 = DIRECTION ( 'NONE',  ( 0.000000000000000000, 1.000000000000000000, -0.000000000000000000 ) ) ;
#17958 = EDGE_CURVE ( 'NONE', #9136, #8404, #9343, .T. ) ;
#17959 = ORIENTED_EDGE ( 'NONE', *, *, #9537, .F. ) ;
#17960 = EDGE_CURVE ( 'NONE', #10840, #2786, #12028, .T. ) ;
#17961 = ORIENTED_EDGE ( 'NONE', *, *, #10104, .T. ) ;
#17962 = AXIS2_PLACEMENT_3D ( 'NONE', #6092, #4775, #16192 ) ;
#17963 = CIRCLE ( 'NONE', #11123, 10.04359719766049430 ) ;
#17964 = ORIENTED_EDGE ( 'NONE', *, *, #3310, .F. ) ;
#17965 = EDGE_CURVE ( 'NONE', #13603, #11807, #6035, .T. ) ;
#17966 = CARTESIAN_POINT ( 'NONE',  ( -54.78701292294434211, 94.21775734381050427, -15.00000000000001421 ) ) ;
#17967 = DIRECTION ( 'NONE',  ( -1.000000000000000000, 3.926781602367242350E-14, 1.692578276882432005E-16 ) ) ;
#17968 = CARTESIAN_POINT ( 'NONE',  ( -71.24615306438084872, 91.68240965456375591, -15.00000000000001421 ) ) ;
#17969 = DIRECTION ( 'NONE',  ( 0.9396926207859097602, 0.3420201433256649381, 4.890320548438455808E-16 ) ) ;
#17970 = AXIS2_PLACEMENT_3D ( 'NONE', #514, #7907, #6298 ) ;
#17971 = CARTESIAN_POINT ( 'NONE',  ( -63.16290507965269541, 75.97988867778799715, -15.00000000000001421 ) ) ;
#17972 = CARTESIAN_POINT ( 'NONE',  ( 0.2573354458087886432, 6.889406814520515177, -1.067197363239279939 ) ) ;
#17973 = ORIENTED_EDGE ( 'NONE', *, *, #6768, .T. ) ;
#17974 = CARTESIAN_POINT ( 'NONE',  ( -71.24615306438106188, 38.27533460456375281, -167.1454815528550739 ) ) ;
#17975 = CARTESIAN_POINT ( 'NONE',  ( -92.59262256747318531, 0.3328663868096687350, 25.00000000000000000 ) ) ;
#17977 = ORIENTED_EDGE ( 'NONE', *, *, #12514, .T. ) ;
#17976 = DIRECTION ( 'NONE',  ( -1.000000000000000000, 5.107025913275718824E-14, 1.387778780781445182E-16 ) ) ;
#17978 = LINE ( 'NONE', #13500, #9040 ) ;
#17979 = CIRCLE ( 'NONE', #17673, 12.49999999999999112 ) ;
#17980 = AXIS2_PLACEMENT_3D ( 'NONE', #14400, #14496, #12752 ) ;
#17981 = ORIENTED_EDGE ( 'NONE', *, *, #12894, .T. ) ;
#17982 = CARTESIAN_POINT ( 'NONE',  ( -68.99615306438083451, 95.64293533166268446, 15.00000000000006928 ) ) ;
#17983 = ORIENTED_EDGE ( 'NONE', *, *, #762, .T. ) ;
#17984 = DIRECTION ( 'NONE',  ( 1.000000000000000000, 0.000000000000000000, 6.950654929607132427E-15 ) ) ;
#17985 = VERTEX_POINT ( 'NONE', #3938 ) ;
#17986 = VECTOR ( 'NONE', #8834, 1000.000000000000000 ) ;
#17987 = VERTEX_POINT ( 'NONE', #6838 ) ;
#17988 = VECTOR ( 'NONE', #10679, 1000.000000000000000 ) ;
#17989 = VECTOR ( 'NONE', #7154, 1000.000000000000000 ) ;
#17990 = DIRECTION ( 'NONE',  ( -1.000000000000000000, -0.000000000000000000, -0.000000000000000000 ) ) ;
#17991 = LINE ( 'NONE', #8364, #4870 ) ;
#17992 = CARTESIAN_POINT ( 'NONE',  ( 124.5381772159375942, -151.5628872026272802, -35.99999999999997158 ) ) ;
#17993 = EDGE_LOOP ( 'NONE', ( #15343, #1303, #5907, #8333 ) ) ;
#17994 = APPLICATION_PROTOCOL_DEFINITION ( 'draft international standard', 'automotive_design', 1998, #7760 ) ;
#17995 = CARTESIAN_POINT ( 'NONE',  ( -60.06546592763100278, -96.08423613455721579, -28.18308811886526755 ) ) ;
#17996 = CARTESIAN_POINT ( 'NONE',  ( -71.24615306438111872, 22.56737135456379661, -15.00000000000001421 ) ) ;
#17997 = ORIENTED_EDGE ( 'NONE', *, *, #10303, .F. ) ;
#17998 = VECTOR ( 'NONE', #131, 1000.000000000000000 ) ;
#17999 = DIRECTION ( 'NONE',  ( 0.000000000000000000, 1.000000000000000000, 0.000000000000000000 ) ) ;
#18000 = DIRECTION ( 'NONE',  ( -0.000000000000000000, 0.000000000000000000, 1.000000000000000000 ) ) ;
#18001 = LINE ( 'NONE', #6134, #3057 ) ;
#18002 = VERTEX_POINT ( 'NONE', #17128 ) ;
#18003 = CARTESIAN_POINT ( 'NONE',  ( -76.15046549741104798, 106.5634658120143570, -26.28507553062743085 ) ) ;
#18004 = CARTESIAN_POINT ( 'NONE',  ( -71.24615306438067819, 144.2006139652292518, -15.00000000000001421 ) ) ;
#18005 = EDGE_LOOP ( 'NONE', ( #10935, #11569, #7973, #16479 ) ) ;
#18006 = CIRCLE ( 'NONE', #8155, 7.500000000000000000 ) ;
#18007 = VECTOR ( 'NONE', #16098, 1000.000000000000000 ) ;
#18008 = DIRECTION ( 'NONE',  ( 0.000000000000000000, 1.000000000000000000, -0.000000000000000000 ) ) ;
#18009 = CARTESIAN_POINT ( 'NONE',  ( -71.24615306438114715, 12.25372266522925457, -167.1454815528550739 ) ) ;
#18010 = ORIENTED_EDGE ( 'NONE', *, *, #7011, .T. ) ;
#18011 = AXIS2_PLACEMENT_3D ( 'NONE', #2300, #12430, #11015 ) ;
#18012 = VERTEX_POINT ( 'NONE', #18162 ) ;
#18013 = CARTESIAN_POINT ( 'NONE',  ( -68.99615306438106188, 29.66948968166269296, 15.00000000000006928 ) ) ;
#18014 = PLANE ( 'NONE',  #693 ) ;
#18015 = ORIENTED_EDGE ( 'NONE', *, *, #5723, .F. ) ;
#18016 = AXIS2_PLACEMENT_3D ( 'NONE', #14566, #14741, #14390 ) ;
#18017 = VECTOR ( 'NONE', #15145, 999.9999999999998863 ) ;
#18018 = DIRECTION ( 'NONE',  ( 0.000000000000000000, 0.000000000000000000, 1.000000000000000000 ) ) ;
#18020 = AXIS2_PLACEMENT_3D ( 'NONE', #3626, #15041, #15229 ) ;
#18019 = CARTESIAN_POINT ( 'NONE',  ( -77.01829067351829394, 77.49513323845336288, 59.15998809532618452 ) ) ;
#18021 = LINE ( 'NONE', #13541, #14716 ) ;
#18022 = DIRECTION ( 'NONE',  ( -1.000000000000000000, 0.000000000000000000, 0.000000000000000000 ) ) ;
#18023 = ORIENTED_EDGE ( 'NONE', *, *, #17937, .F. ) ;
#18024 = EDGE_CURVE ( 'NONE', #5717, #15520, #15454, .T. ) ;
#18025 = DIRECTION ( 'NONE',  ( 0.000000000000000000, 0.000000000000000000, 1.000000000000000000 ) ) ;
#18026 = LINE ( 'NONE', #5209, #9431 ) ;
#18027 = PLANE ( 'NONE',  #7337 ) ;
#18028 = CARTESIAN_POINT ( 'NONE',  ( -1.859018761987631274, 12.02839362309843274, -46.70372576070108295 ) ) ;
#18029 = CYLINDRICAL_SURFACE ( 'NONE', #353, 12.49999999999999645 ) ;
#18030 = VERTEX_POINT ( 'NONE', #2833 ) ;
#18031 = DIRECTION ( 'NONE',  ( 0.9396926207859171987, 0.3420201433256445100, 4.890320548438495251E-16 ) ) ;
#18032 = CARTESIAN_POINT ( 'NONE',  ( -60.19468178563425198, -91.08423613455723000, 39.14310232490466035 ) ) ;
#18033 = VERTEX_POINT ( 'NONE', #15646 ) ;
#18034 = DIRECTION ( 'NONE',  ( 0.000000000000000000, 0.000000000000000000, 1.000000000000000000 ) ) ;
#18035 = PLANE ( 'NONE',  #7486 ) ;
#18036 = AXIS2_PLACEMENT_3D ( 'NONE', #17433, #17253, #13070 ) ;
#18037 = SURFACE_STYLE_FILL_AREA ( #3730 ) ;
#18038 = ORIENTED_EDGE ( 'NONE', *, *, #4913, .T. ) ;
#18039 = ORIENTED_EDGE ( 'NONE', *, *, #17366, .T. ) ;
#18040 = LINE ( 'NONE', #9345, #15651 ) ;
#18041 = AXIS2_PLACEMENT_3D ( 'NONE', #4173, #15694, #3983 ) ;
#18042 = ORIENTED_EDGE ( 'NONE', *, *, #2537, .T. ) ;
#18043 = FACE_OUTER_BOUND ( 'NONE', #11908, .T. ) ;
#18044 = LINE ( 'NONE', #16270, #2179 ) ;
#18045 = CARTESIAN_POINT ( 'NONE',  ( -66.20417287045881949, 57.28139718322722018, -28.00000000000000711 ) ) ;
#18046 = EDGE_CURVE ( 'NONE', #9806, #17985, #5709, .T. ) ;
#18047 = CARTESIAN_POINT ( 'NONE',  ( -71.24615306438097662, 59.37761241522920841, -167.1454815528550739 ) ) ;
#18048 = AXIS2_PLACEMENT_3D ( 'NONE', #8584, #8398, #4181 ) ;
#18049 = DIRECTION ( 'NONE',  ( 0.000000000000000000, 0.000000000000000000, 1.000000000000000000 ) ) ;
#18050 = CIRCLE ( 'NONE', #1916, 34.36884788726141693 ) ;
#18051 = CARTESIAN_POINT ( 'NONE',  ( -102.5926225674731853, 102.8748711238780373, 20.00000000000000355 ) ) ;
#18052 = PRODUCT_DEFINITION_SHAPE ( 'NONE', 'NONE',  #1557 ) ;
#18053 = ORIENTED_EDGE ( 'NONE', *, *, #6641, .T. ) ;
#18054 = CARTESIAN_POINT ( 'NONE',  ( -71.24615306438079188, 112.7846874652292399, -167.1454815528550739 ) ) ;
#18055 = CARTESIAN_POINT ( 'NONE',  ( -68.99615306438103346, 32.81108233166271759, -167.1454815528550739 ) ) ;
#18056 = EDGE_LOOP ( 'NONE', ( #16841, #6440, #15639, #3916 ) ) ;
#18057 = VECTOR ( 'NONE', #14527, 1000.000000000000000 ) ;
#18058 = EDGE_CURVE ( 'NONE', #5881, #9725, #15006, .T. ) ;
#18059 = LINE ( 'NONE', #7860, #7335 ) ;
#18060 = CARTESIAN_POINT ( 'NONE',  ( -70.06856178257687873, 57.88796029049330372, 22.35917033480642502 ) ) ;
#18061 = ORIENTED_EDGE ( 'NONE', *, *, #13159, .T. ) ;
#18062 = EDGE_LOOP ( 'NONE', ( #17959, #3369, #1498, #4230 ) ) ;
#18063 = CIRCLE ( 'NONE', #3735, 2.168074330099287295 ) ;
#18064 = ADVANCED_FACE ( 'NONE', ( #8544 ), #2554, .F. ) ;
#18065 = VECTOR ( 'NONE', #17343, 1000.000000000000000 ) ;
#18066 = VECTOR ( 'NONE', #12469, 1000.000000000000000 ) ;
#18067 = VERTEX_POINT ( 'NONE', #18259 ) ;
#18068 = UNCERTAINTY_MEASURE_WITH_UNIT (LENGTH_MEASURE( 1.000000000000000082E-05 ), #13261, 'distance_accuracy_value', 'NONE');
#18069 = EDGE_CURVE ( 'NONE', #3821, #8277, #14248, .T. ) ;
#18070 = CYLINDRICAL_SURFACE ( 'NONE', #5216, 18.23991632971910803 ) ;
#18071 = PLANE ( 'NONE',  #371 ) ;
#18072 = EDGE_CURVE ( 'NONE', #9948, #3784, #14442, .T. ) ;
#18073 = PLANE ( 'NONE',  #7297 ) ;
#18074 = CARTESIAN_POINT ( 'NONE',  ( -57.08002265617300708, 84.22855780814606419, 37.50000000000000000 ) ) ;
#18075 = EDGE_CURVE ( 'NONE', #13442, #17198, #12558, .T. ) ;
#18076 = CARTESIAN_POINT ( 'NONE',  ( 95.45835937779683888, -32.62665103886254059, 7.000000000000010658 ) ) ;
#18077 = LINE ( 'NONE', #12672, #13211 ) ;
#18078 = ORIENTED_EDGE ( 'NONE', *, *, #15322, .F. ) ;
#18079 = AXIS2_PLACEMENT_3D ( 'NONE', #10312, #13119, #4593 ) ;
#18080 = DIRECTION ( 'NONE',  ( 1.156482317317869999E-16, 0.000000000000000000, 1.000000000000000000 ) ) ;
#18081 = LINE ( 'NONE', #2264, #10795 ) ;
#18083 = VERTEX_POINT ( 'NONE', #5431 ) ;
#18082 = CARTESIAN_POINT ( 'NONE',  ( -78.12361985383350316, 84.72841810161551734, 70.00000000000001421 ) ) ;
#18084 = DIRECTION ( 'NONE',  ( -0.9396926207859084279, 0.3420201433256686574, -4.890320548438448905E-16 ) ) ;
#18085 = CIRCLE ( 'NONE', #4045, 7.168074330098860969 ) ;
#18086 = VECTOR ( 'NONE', #13262, 1000.000000000000000 ) ;
#18087 = CARTESIAN_POINT ( 'NONE',  ( -71.24615306438106188, 38.27533460456375281, -167.1454815528550739 ) ) ;
#18088 = VERTEX_POINT ( 'NONE', #11436 ) ;
#18089 = EDGE_CURVE ( 'NONE', #15247, #845, #16512, .T. ) ;
#18090 = ADVANCED_FACE ( 'NONE', ( #11341 ), #8339, .T. ) ;
#18091 = ADVANCED_FACE ( 'NONE', ( #5537 ), #11261, .T. ) ;
#18092 = FACE_OUTER_BOUND ( 'NONE', #16159, .T. ) ;
#18093 = ORIENTED_EDGE ( 'NONE', *, *, #9981, .F. ) ;
#18094 = EDGE_CURVE ( 'NONE', #850, #17620, #7276, .T. ) ;
#18095 = ORIENTED_EDGE ( 'NONE', *, *, #3689, .T. ) ;
#18096 = CIRCLE ( 'NONE', #14796, 4.599999999999992539 ) ;
#18097 = CARTESIAN_POINT ( 'NONE',  ( -92.59262256747319952, 60.58224449241411946, 25.00000000000000000 ) ) ;
#18098 = CARTESIAN_POINT ( 'NONE',  ( -68.30128029835485393, 78.72098330317788850, 15.00000000000006928 ) ) ;
#18099 = CARTESIAN_POINT ( 'NONE',  ( -71.24615306438114715, 9.112130015229229940, -167.1454815528550739 ) ) ;
#18100 = ORIENTED_EDGE ( 'NONE', *, *, #16825, .F. ) ;
#18101 = APPLICATION_PROTOCOL_DEFINITION ( 'draft international standard', 'automotive_design', 1998, #15160 ) ;
#18102 = EDGE_CURVE ( 'NONE', #12836, #11918, #12936, .T. ) ;
#18103 = CARTESIAN_POINT ( 'NONE',  ( 11.11671913661698774, 6.304244514274031097, -48.62687381527162955 ) ) ;
#18104 = EDGE_CURVE ( 'NONE', #18456, #18220, #3262, .T. ) ;
#18105 = DIRECTION ( 'NONE',  ( 1.000000000000000000, 0.000000000000000000, 0.000000000000000000 ) ) ;
#18106 = EDGE_LOOP ( 'NONE', ( #15824, #3701, #4758, #18173 ) ) ;
#18107 = PRESENTATION_STYLE_ASSIGNMENT (( #12411 ) ) ;
#18108 = DIRECTION ( 'NONE',  ( 1.000000000000000000, 0.000000000000000000, 5.077734830647302671E-16 ) ) ;
#18109 = DIRECTION ( 'NONE',  ( 0.3420201433256686574, -0.9396926207859084279, 0.000000000000000000 ) ) ;
#18110 = EDGE_LOOP ( 'NONE', ( #12265, #5459, #14599, #1973 ) ) ;
#18111 = FACE_OUTER_BOUND ( 'NONE', #11147, .T. ) ;
#18112 = CARTESIAN_POINT ( 'NONE',  ( -70.71978124295708312, -111.0842361345572158, 22.52877280353970235 ) ) ;
#18113 = ORIENTED_EDGE ( 'NONE', *, *, #8510, .F. ) ;
#18114 = DIRECTION ( 'NONE',  ( 0.000000000000000000, 0.000000000000000000, -1.000000000000000000 ) ) ;
#18115 = DIRECTION ( 'NONE',  ( 0.000000000000000000, 0.000000000000000000, 1.000000000000000000 ) ) ;
#18116 = VERTEX_POINT ( 'NONE', #7576 ) ;
#18117 = ORIENTED_EDGE ( 'NONE', *, *, #6030, .T. ) ;
#18118 = ORIENTED_EDGE ( 'NONE', *, *, #7237, .T. ) ;
#18119 = DIRECTION ( 'NONE',  ( 0.3420201433256675472, 0.9396926207859088720, -0.000000000000000000 ) ) ;
#18120 = LINE ( 'NONE', #16692, #410 ) ;
#18121 = ADVANCED_FACE ( 'NONE', ( #3005 ), #375, .F. ) ;
#18122 = ORIENTED_EDGE ( 'NONE', *, *, #11958, .F. ) ;
#18123 = DIRECTION ( 'NONE',  ( 0.000000000000000000, 0.000000000000000000, 1.000000000000000000 ) ) ;
#18124 = DIRECTION ( 'NONE',  ( 0.000000000000000000, 0.000000000000000000, 1.000000000000000000 ) ) ;
#18125 = DIRECTION ( 'NONE',  ( 0.000000000000000000, 0.000000000000000000, -1.000000000000000000 ) ) ;
#18126 = DIRECTION ( 'NONE',  ( 1.000000000000000000, 0.000000000000000000, 0.000000000000000000 ) ) ;
#18127 = VERTEX_POINT ( 'NONE', #471 ) ;
#18128 = LINE ( 'NONE', #2500, #917 ) ;
#18129 = CARTESIAN_POINT ( 'NONE',  ( -68.99615306438077766, 111.3508985816626335, -15.00000000000001421 ) ) ;
#18130 = CARTESIAN_POINT ( 'NONE',  ( -57.08002265617300708, 84.22855780814606419, -15.00000000000001421 ) ) ;
#18131 = CARTESIAN_POINT ( 'NONE',  ( -31.74593505105995916, -91.08423613455721579, 10.65431531532568599 ) ) ;
#18132 = CARTESIAN_POINT ( 'NONE',  ( 15.23320273812466041, -19.34983604512934363, 54.79921157549236455 ) ) ;
#18133 = ORIENTED_EDGE ( 'NONE', *, *, #11667, .T. ) ;
#18134 = LINE ( 'NONE', #5308, #2234 ) ;
#18135 = CARTESIAN_POINT ( 'NONE',  ( -64.09091675476031469, -93.09900487505517219, 43.93281256380674193 ) ) ;
#18136 = ORIENTED_EDGE ( 'NONE', *, *, #8011, .F. ) ;
#18137 = CYLINDRICAL_SURFACE ( 'NONE', #9275, 11.04359719766049430 ) ;
#18138 = DIRECTION ( 'NONE',  ( -0.3197242186372270534, 0.9475106458593564041, 0.000000000000000000 ) ) ;
#18139 = ORIENTED_EDGE ( 'NONE', *, *, #3925, .F. ) ;
#18140 = EDGE_CURVE ( 'NONE', #3197, #18067, #8893, .T. ) ;
#18141 = VERTEX_POINT ( 'NONE', #4666 ) ;
#18142 = B_SPLINE_CURVE_WITH_KNOTS ( 'NONE', 3,
 ( #9283, #12183, #17873, #15159, #18463, #9842, #14057, #6944 ),
 .UNSPECIFIED., .F., .F.,
 ( 4, 2, 2, 4 ),
 ( 0.003797433802554483605, 0.004743183970586266514, 0.005688934138618047254, 0.007580434474681613070 ),
 .UNSPECIFIED. ) ;
#18143 = DIRECTION ( 'NONE',  ( -1.000000000000000000, 0.000000000000000000, 0.000000000000000000 ) ) ;
#18144 = EDGE_CURVE ( 'NONE', #11961, #14807, #3094, .T. ) ;
#18145 = ORIENTED_EDGE ( 'NONE', *, *, #11845, .F. ) ;
#18146 = LINE ( 'NONE', #1318, #14787 ) ;
#18147 = CARTESIAN_POINT ( 'NONE',  ( 0.000000000000000000, -91.08423613455721579, -5.654315315325675328 ) ) ;
#18148 = FACE_OUTER_BOUND ( 'NONE', #171, .T. ) ;
#18149 = LINE ( 'NONE', #6824, #14056 ) ;
#18150 = CARTESIAN_POINT ( 'NONE',  ( -50.06979403241810900, 50.58224449241409104, 26.91246033477412425 ) ) ;
#18151 = CARTESIAN_POINT ( 'NONE',  ( -68.99615306438091977, 74.26664263813029265, -167.1454815528550739 ) ) ;
#18152 = EDGE_LOOP ( 'NONE', ( #16614, #17612, #13346, #14429 ) ) ;
#18153 = CARTESIAN_POINT ( 'NONE',  ( -47.88529808651028929, 78.55081803573747834, 15.00000000000006928 ) ) ;
#18154 = DIRECTION ( 'NONE',  ( -0.000000000000000000, 1.000000000000000000, 0.000000000000000000 ) ) ;
#18155 = ORIENTED_EDGE ( 'NONE', *, *, #8360, .T. ) ;
#18156 = CARTESIAN_POINT ( 'NONE',  ( -25.97029152202262026, -94.42547236494613117, -5.919112892686000826 ) ) ;
#18157 = DIRECTION ( 'NONE',  ( 1.000000000000000000, 0.000000000000000000, 0.000000000000000000 ) ) ;
#18158 = EDGE_LOOP ( 'NONE', ( #17504, #17863, #2914, #5978, #5944 ) ) ;
#18159 = VERTEX_POINT ( 'NONE', #6148 ) ;
#18160 = ORIENTED_EDGE ( 'NONE', *, *, #7284, .T. ) ;
#18161 = LINE ( 'NONE', #5332, #2813 ) ;
#18162 = CARTESIAN_POINT ( 'NONE',  ( 98.04320049944426785, 84.22855780814606419, 72.88004356723772048 ) ) ;
#18163 = CARTESIAN_POINT ( 'NONE',  ( -51.34465738200551499, 92.72253132893560235, 15.00000000000006928 ) ) ;
#18164 = CARTESIAN_POINT ( 'NONE',  ( -46.89970808030100358, 83.04399200740388665, -15.00000000000001421 ) ) ;
#18165 = EDGE_CURVE ( 'NONE', #17387, #13170, #4579, .T. ) ;
#18166 = DIRECTION ( 'NONE',  ( -1.000000000000000000, -0.000000000000000000, -0.000000000000000000 ) ) ;
#18167 = FACE_OUTER_BOUND ( 'NONE', #8167, .T. ) ;
#18168 = DIRECTION ( 'NONE',  ( 1.000000000000000000, -0.000000000000000000, -0.000000000000000000 ) ) ;
#18169 = ORIENTED_EDGE ( 'NONE', *, *, #12610, .T. ) ;
#18170 = CARTESIAN_POINT ( 'NONE',  ( -67.37337372105014310, 111.7354893787529022, 22.91102204468130310 ) ) ;
#18171 = CARTESIAN_POINT ( 'NONE',  ( -98.90286936182231159, -111.0842361345572158, -5.654315315325883162 ) ) ;
#18173 = ORIENTED_EDGE ( 'NONE', *, *, #15181, .F. ) ;
#18172 = CARTESIAN_POINT ( 'NONE',  ( -78.03437486056226646, 86.17903909013998032, 69.74613384661780913 ) ) ;
#18174 = FACE_OUTER_BOUND ( 'NONE', #11829, .T. ) ;
#18175 = DIRECTION ( 'NONE',  ( 0.000000000000000000, 5.551115123125748189E-17, 1.000000000000000000 ) ) ;
#18176 = VECTOR ( 'NONE', #11832, 1000.000000000000000 ) ;
#18177 = ORIENTED_EDGE ( 'NONE', *, *, #15441, .F. ) ;
#18178 = DIRECTION ( 'NONE',  ( 0.9396926207859043201, 0.3420201433256802037, 0.000000000000000000 ) ) ;
#18179 = VERTEX_POINT ( 'NONE', #17483 ) ;
#18180 = EDGE_CURVE ( 'NONE', #5451, #5525, #13292, .T. ) ;
#18181 = EDGE_CURVE ( 'NONE', #1895, #4188, #7218, .T. ) ;
#18182 = ORIENTED_EDGE ( 'NONE', *, *, #14845, .T. ) ;
#18183 = PRESENTATION_STYLE_ASSIGNMENT (( #15665 ) ) ;
#18184 = AXIS2_PLACEMENT_3D ( 'NONE', #6352, #484, #3368 ) ;
#18185 = FACE_OUTER_BOUND ( 'NONE', #17765, .T. ) ;
#18186 = LINE ( 'NONE', #14170, #3344 ) ;
#18187 = EDGE_CURVE ( 'NONE', #9316, #18141, #1509, .T. ) ;
#18188 = VERTEX_POINT ( 'NONE', #4403 ) ;
#18189 = DIRECTION ( 'NONE',  ( 1.000000000000000000, 0.000000000000000000, 0.000000000000000000 ) ) ;
#18190 = EDGE_CURVE ( 'NONE', #17894, #16349, #8982, .T. ) ;
#18191 = CARTESIAN_POINT ( 'NONE',  ( -29.09351669014244379, -91.53392936304807392, 8.561724358915446587 ) ) ;
#18192 = CARTESIAN_POINT ( 'NONE',  ( -71.24615306438103346, 47.70011255456374499, 15.00000000000006928 ) ) ;
#18193 = EDGE_LOOP ( 'NONE', ( #6437, #12793, #17477, #9195 ) ) ;
#18194 = CYLINDRICAL_SURFACE ( 'NONE', #15570, 10.24899999999999345 ) ;
#18195 = DIRECTION ( 'NONE',  ( -0.000000000000000000, -1.000000000000000000, -0.000000000000000000 ) ) ;
#18196 = FACE_OUTER_BOUND ( 'NONE', #17148, .T. ) ;
#18197 = ORIENTED_EDGE ( 'NONE', *, *, #16029, .T. ) ;
#18198 = CARTESIAN_POINT ( 'NONE',  ( -61.98611128973170992, 74.59995546124152099, -15.00000000000001421 ) ) ;
#18199 = DIRECTION ( 'NONE',  ( 0.000000000000000000, 0.000000000000000000, 1.000000000000000000 ) ) ;
#18200 = ORIENTED_EDGE ( 'NONE', *, *, #5918, .T. ) ;
#18201 = EDGE_CURVE ( 'NONE', #1024, #1562, #5155, .T. ) ;
#18202 = LINE ( 'NONE', #5473, #12740 ) ;
#18204 = EDGE_CURVE ( 'NONE', #8426, #15763, #7311, .T. ) ;
#18203 = VECTOR ( 'NONE', #1730, 1000.000000000000000 ) ;
#18205 = LINE ( 'NONE', #11098, #17751 ) ;
#18206 = ORIENTED_EDGE ( 'NONE', *, *, #5730, .F. ) ;
#18207 = EDGE_CURVE ( 'NONE', #10434, #2512, #13107, .T. ) ;
#18208 = EDGE_CURVE ( 'NONE', #10713, #4400, #202, .T. ) ;
#18209 = PRODUCT_DEFINITION_SHAPE ( 'NONE', 'NONE',  #18523 ) ;
#18210 = ORIENTED_EDGE ( 'NONE', *, *, #1425, .F. ) ;
#18211 = CARTESIAN_POINT ( 'NONE',  ( -70.71978124295696944, -111.0842361345572158, 5.204170427930421283E-15 ) ) ;
#18212 = CARTESIAN_POINT ( 'NONE',  ( -71.24615306438109030, 27.96168591522921076, -167.1454815528550739 ) ) ;
#18213 = EDGE_CURVE ( 'NONE', #18272, #8741, #4486, .T. ) ;
#18214 = VERTEX_POINT ( 'NONE', #6065 ) ;
#18215 = DIRECTION ( 'NONE',  ( -5.204170427930409450E-16, 0.000000000000000000, 1.000000000000000000 ) ) ;
#18216 = CARTESIAN_POINT ( 'NONE',  ( -68.99615306438106188, 29.66948968166269651, -15.00000000000001421 ) ) ;
#18217 = CARTESIAN_POINT ( 'NONE',  ( -34.72861478725227613, 45.17254440751388245, 30.47173447583816852 ) ) ;
#18218 = CIRCLE ( 'NONE', #17603, 4.600000000000006750 ) ;
#18219 = DIRECTION ( 'NONE',  ( 0.000000000000000000, 1.000000000000000000, 0.000000000000000000 ) ) ;
#18220 = VERTEX_POINT ( 'NONE', #10202 ) ;
#18221 = CARTESIAN_POINT ( 'NONE',  ( -46.83322972390671879, 84.01587117655466841, 15.00000000000009592 ) ) ;
#18222 = CIRCLE ( 'NONE', #10435, 10.65431531532567888 ) ;
#18223 = DIRECTION ( 'NONE',  ( 0.000000000000000000, 0.000000000000000000, 1.000000000000000000 ) ) ;
#18224 = CARTESIAN_POINT ( 'NONE',  ( -57.08002265617300708, 84.22855780814606419, -15.00000000000001421 ) ) ;
#18225 = CARTESIAN_POINT ( 'NONE',  ( -46.38449965345759551, 85.77305660501679085, 15.00000000000009592 ) ) ;
#18226 = CARTESIAN_POINT ( 'NONE',  ( -0.3127821567423632598, 28.68880187506458412, 39.62697943036548764 ) ) ;
#18227 = ORIENTED_EDGE ( 'NONE', *, *, #9291, .T. ) ;
#18228 = FACE_OUTER_BOUND ( 'NONE', #5367, .T. ) ;
#18229 = LINE ( 'NONE', #4617, #5986 ) ;
#18230 = CARTESIAN_POINT ( 'NONE',  ( -35.03642545851250389, 84.22855780814606419, -124.8487082408420861 ) ) ;
#18231 = ORIENTED_EDGE ( 'NONE', *, *, #9537, .T. ) ;
#18232 = CIRCLE ( 'NONE', #13148, 7.500000000000000000 ) ;
#18233 = ORIENTED_EDGE ( 'NONE', *, *, #9237, .T. ) ;
#18234 = VECTOR ( 'NONE', #14151, 1000.000000000000000 ) ;
#18235 = DIRECTION ( 'NONE',  ( 1.000000000000000000, 0.000000000000000000, 0.000000000000000000 ) ) ;
#18236 = CARTESIAN_POINT ( 'NONE',  ( -59.35080917176598092, 94.79374675277695417, -167.1454815528550739 ) ) ;
#18237 = CARTESIAN_POINT ( 'NONE',  ( -75.21640136043859570, 61.12840431439423838, 24.01061398482676879 ) ) ;
#18238 = CARTESIAN_POINT ( 'NONE',  ( -66.51364668169601657, 56.41604328733773599, -28.00000000000000355 ) ) ;
#18239 = ORIENTED_EDGE ( 'NONE', *, *, #6156, .F. ) ;
#18240 = DIRECTION ( 'NONE',  ( -0.9396926207859084279, 0.3420201433256686574, -4.890320548438448905E-16 ) ) ;
#18241 = LINE ( 'NONE', #16634, #4915 ) ;
#18242 = DIRECTION ( 'NONE',  ( -1.000000000000000000, 0.000000000000000000, 0.000000000000000000 ) ) ;
#18243 = VERTEX_POINT ( 'NONE', #1869 ) ;
#18244 = VECTOR ( 'NONE', #15528, 1000.000000000000000 ) ;
#18245 = CIRCLE ( 'NONE', #8974, 12.29357405616490695 ) ;
#18246 = VECTOR ( 'NONE', #10656, 1000.000000000000000 ) ;
#18247 = CARTESIAN_POINT ( 'NONE',  ( -71.24615306438080609, 107.3903729045637192, -15.00000000000001421 ) ) ;
#18248 = ORIENTED_EDGE ( 'NONE', *, *, #2552, .F. ) ;
#18249 = CARTESIAN_POINT ( 'NONE',  ( -64.22944241949029731, 91.57211267264378307, -15.00000000000001421 ) ) ;
#18250 = FACE_OUTER_BOUND ( 'NONE', #12410, .T. ) ;
#18251 = VERTEX_POINT ( 'NONE', #17564 ) ;
#18252 = ORIENTED_EDGE ( 'NONE', *, *, #3376, .T. ) ;
#18253 = VECTOR ( 'NONE', #9162, 1000.000000000000000 ) ;
#18254 = CIRCLE ( 'NONE', #16440, 11.04359719766050141 ) ;
#18255 = ORIENTED_EDGE ( 'NONE', *, *, #16546, .T. ) ;
#18256 = UNCERTAINTY_MEASURE_WITH_UNIT (LENGTH_MEASURE( 1.000000000000000082E-05 ), #11672, 'distance_accuracy_value', 'NONE');
#18257 = VECTOR ( 'NONE', #9995, 1000.000000000000000 ) ;
#18258 = DIRECTION ( 'NONE',  ( 1.000000000000000000, 0.000000000000000000, 0.000000000000000000 ) ) ;
#18259 = CARTESIAN_POINT ( 'NONE',  ( -68.99615306438097662, 61.70027203813028649, -15.00000000000001421 ) ) ;
#18260 = LINE ( 'NONE', #3843, #16254 ) ;
#18261 = CYLINDRICAL_SURFACE ( 'NONE', #16814, 26.04359719766049253 ) ;
#18262 = LINE ( 'NONE', #10034, #15833 ) ;
#18263 = CARTESIAN_POINT ( 'NONE',  ( -107.5926225674731853, 110.5691553257988460, -26.35917033480641436 ) ) ;
#18264 = ORIENTED_EDGE ( 'NONE', *, *, #8942, .F. ) ;
#18265 = DIRECTION ( 'NONE',  ( 0.000000000000000000, 0.000000000000000000, 1.000000000000000000 ) ) ;
#18266 = CARTESIAN_POINT ( 'NONE',  ( -70.71978124295708312, -96.08423613455721579, 28.18308811886538479 ) ) ;
#18268 = ORIENTED_EDGE ( 'NONE', *, *, #11071, .T. ) ;
#18267 = DIRECTION ( 'NONE',  ( 1.000000000000000000, 0.000000000000000000, 0.000000000000000000 ) ) ;
#18269 = VECTOR ( 'NONE', #6581, 1000.000000000000000 ) ;
#18270 = CARTESIAN_POINT ( 'NONE',  ( -66.56323152365561668, 80.34130291867722917, -15.00000000000001243 ) ) ;
#18271 = DIRECTION ( 'NONE',  ( 0.000000000000000000, 0.000000000000000000, 1.000000000000000000 ) ) ;
#18272 = VERTEX_POINT ( 'NONE', #4746 ) ;
#18273 = AXIS2_PLACEMENT_3D ( 'NONE', #5651, #17068, #4347 ) ;
#18274 = VECTOR ( 'NONE', #14720, 999.9999999999998863 ) ;
#18275 = CYLINDRICAL_SURFACE ( 'NONE', #1448, 4.600000000000006750 ) ;
#18276 = ORIENTED_EDGE ( 'NONE', *, *, #13267, .T. ) ;
#18277 = EDGE_CURVE ( 'NONE', #11275, #9222, #18006, .T. ) ;
#18278 = ORIENTED_EDGE ( 'NONE', *, *, #15578, .T. ) ;
#18279 = AXIS2_PLACEMENT_3D ( 'NONE', #8161, #1068, #6760 ) ;
#18280 = FILL_AREA_STYLE ('',( #6774 ) ) ;
#18281 = CARTESIAN_POINT ( 'NONE',  ( -48.98198201484814263, 93.75072866207695199, 15.00000000000006928 ) ) ;
#18282 = CARTESIAN_POINT ( 'NONE',  ( -60.18936887439735273, 72.12145385653096241, 15.00000000000006928 ) ) ;
#18283 = ORIENTED_EDGE ( 'NONE', *, *, #15403, .T. ) ;
#18284 = APPLICATION_PROTOCOL_DEFINITION ( 'draft international standard', 'automotive_design', 1998, #8853 ) ;
#18285 = AXIS2_PLACEMENT_3D ( 'NONE', #13681, #5440, #13775 ) ;
#18286 = ORIENTED_EDGE ( 'NONE', *, *, #12137, .F. ) ;
#18287 = CARTESIAN_POINT ( 'NONE',  ( 15.23320273812466041, -19.34983604512935429, 57.00000000000000000 ) ) ;
#18288 = EDGE_CURVE ( 'NONE', #2703, #1662, #13370, .T. ) ;
#18289 = DIRECTION ( 'NONE',  ( 0.000000000000000000, 0.000000000000000000, 1.000000000000000000 ) ) ;
#18290 = ORIENTED_EDGE ( 'NONE', *, *, #128, .F. ) ;
#18291 = CARTESIAN_POINT ( 'NONE',  ( -57.08002265617300708, 84.22855780814606419, -167.1454815528550739 ) ) ;
#18292 = CARTESIAN_POINT ( 'NONE',  ( -71.24615306438120399, -0.3126479347707321610, 15.00000000000006928 ) ) ;
#18293 = EDGE_CURVE ( 'NONE', #5859, #11918, #15045, .T. ) ;
#18294 = DIRECTION ( 'NONE',  ( 0.000000000000000000, 0.000000000000000000, 1.000000000000000000 ) ) ;
#18295 = ORIENTED_EDGE ( 'NONE', *, *, #16401, .F. ) ;
#18296 = CARTESIAN_POINT ( 'NONE',  ( -68.99615306438106188, 29.66948968166269296, -15.00000000000001421 ) ) ;
#18297 = DIRECTION ( 'NONE',  ( -1.000000000000000000, -0.000000000000000000, -6.950654929607132427E-15 ) ) ;
#18298 = ORIENTED_EDGE ( 'NONE', *, *, #11228, .T. ) ;
#18299 = AXIS2_PLACEMENT_3D ( 'NONE', #1654, #12896, #68 ) ;
#18300 = LINE ( 'NONE', #9587, #10324 ) ;
#18301 = EDGE_CURVE ( 'NONE', #2247, #2087, #11458, .T. ) ;
#18302 = ADVANCED_FACE ( 'NONE', ( #17768 ), #15138, .T. ) ;
#18303 = CARTESIAN_POINT ( 'NONE',  ( -66.21794066256015299, 56.31741075272766039, -27.07314213088852739 ) ) ;
#18304 = VECTOR ( 'NONE', #10552, 1000.000000000000000 ) ;
#18305 = ORIENTED_EDGE ( 'NONE', *, *, #4285, .F. ) ;
#18306 = EDGE_CURVE ( 'NONE', #12513, #9457, #928, .T. ) ;
#18307 = ORIENTED_EDGE ( 'NONE', *, *, #3858, .F. ) ;
#18308 = CARTESIAN_POINT ( 'NONE',  ( -68.99615306438111872, 10.81993378166265529, -167.1454815528550739 ) ) ;
#18309 = VECTOR ( 'NONE', #218, 1000.000000000000000 ) ;
#18310 = ORIENTED_EDGE ( 'NONE', *, *, #8452, .F. ) ;
#18311 = EDGE_CURVE ( 'NONE', #13644, #11558, #6529, .T. ) ;
#18312 = CARTESIAN_POINT ( 'NONE',  ( 15.23320273812466041, -19.34983604512934363, -3.000000000000000000 ) ) ;
#18313 = LINE ( 'NONE', #5486, #5934 ) ;
#18314 = CARTESIAN_POINT ( 'NONE',  ( -7.963671022379969600, 22.16714537965745890, 42.62291292524223252 ) ) ;
#18315 = EDGE_CURVE ( 'NONE', #12217, #13601, #3353, .T. ) ;
#18316 = FACE_OUTER_BOUND ( 'NONE', #372, .T. ) ;
#18317 = ORIENTED_EDGE ( 'NONE', *, *, #11231, .T. ) ;
#18318 = EDGE_CURVE ( 'NONE', #10530, #12457, #10251, .T. ) ;
#18319 = DIRECTION ( 'NONE',  ( 0.000000000000000000, 0.000000000000000000, -1.000000000000000000 ) ) ;
#18320 = CIRCLE ( 'NONE', #12658, 10.24900000000001477 ) ;
#18321 = DIRECTION ( 'NONE',  ( 0.000000000000000000, 3.469446951953617344E-15, 1.000000000000000000 ) ) ;
#18322 = CARTESIAN_POINT ( 'NONE',  ( -57.08002265617300708, 84.22855780814606419, -167.1454815528550739 ) ) ;
#18323 = EDGE_CURVE ( 'NONE', #11131, #16032, #18044, .T. ) ;
#18324 = CARTESIAN_POINT ( 'NONE',  ( -68.99615306438091977, 74.26664263813029265, -167.1454815528550739 ) ) ;
#18325 = DIRECTION ( 'NONE',  ( -1.119176436114069332E-16, 1.000000000000000000, 0.000000000000000000 ) ) ;
#18326 = VERTEX_POINT ( 'NONE', #7667 ) ;
#18327 = DIRECTION ( 'NONE',  ( -0.000000000000000000, -1.000000000000000000, -0.000000000000000000 ) ) ;
#18328 = CARTESIAN_POINT ( 'NONE',  ( -171.0109138863553824, 84.22855780814606419, 62.50000000000001421 ) ) ;
#18329 = EDGE_CURVE ( 'NONE', #14197, #3236, #17942, .T. ) ;
#18330 = AXIS2_PLACEMENT_3D ( 'NONE', #15878, #11673, #13351 ) ;
#18331 = EDGE_CURVE ( 'NONE', #11747, #7063, #6052, .T. ) ;
#18332 = FACE_OUTER_BOUND ( 'NONE', #7364, .T. ) ;
#18333 = ADVANCED_FACE ( 'NONE', ( #14857 ), #5127, .T. ) ;
#18334 = LINE ( 'NONE', #5679, #16735 ) ;
#18335 = VERTEX_POINT ( 'NONE', #16351 ) ;
#18336 = ORIENTED_EDGE ( 'NONE', *, *, #9742, .F. ) ;
#18337 = VECTOR ( 'NONE', #5888, 1000.000000000000000 ) ;
#18338 = AXIS2_PLACEMENT_3D ( 'NONE', #6949, #18373, #15656 ) ;
#18339 = AXIS2_PLACEMENT_3D ( 'NONE', #11508, #343, #1840 ) ;
#18340 = CARTESIAN_POINT ( 'NONE',  ( -45.21333244822126574, 88.15687341518456321, 15.00000000000006928 ) ) ;
#18341 = ORIENTED_EDGE ( 'NONE', *, *, #6649, .T. ) ;
#18342 = CARTESIAN_POINT ( 'NONE',  ( -50.41499038512538533, 117.9449492212793302, 0.000000000000000000 ) ) ;
#18343 = CARTESIAN_POINT ( 'NONE',  ( -64.09025127992791226, 117.8748711238780373, 35.00000000000000000 ) ) ;
#18344 = CARTESIAN_POINT ( 'NONE',  ( -62.92154743286826601, -91.96845925178435266, -42.55229934223195443 ) ) ;
#18345 = EDGE_LOOP ( 'NONE', ( #482, #4772, #2952, #3326 ) ) ;
#18346 = CARTESIAN_POINT ( 'NONE',  ( -66.34489626515157568, 111.6204860916741239, -28.00000000000000000 ) ) ;
#18347 = DIRECTION ( 'NONE',  ( 0.000000000000000000, -5.551115123125747573E-17, -1.000000000000000000 ) ) ;
#18348 = EDGE_CURVE ( 'NONE', #646, #17620, #3538, .T. ) ;
#18349 = DIRECTION ( 'NONE',  ( 0.000000000000000000, 1.000000000000000000, 0.000000000000000000 ) ) ;
#18350 = DIRECTION ( 'NONE',  ( 0.000000000000000000, 0.000000000000000000, 1.000000000000000000 ) ) ;
#18351 = ORIENTED_EDGE ( 'NONE', *, *, #9835, .T. ) ;
#18352 = ADVANCED_FACE ( 'NONE', ( #14941 ), #13464, .T. ) ;
#18353 = AXIS2_PLACEMENT_3D ( 'NONE', #5230, #15332, #6531 ) ;
#18354 = VECTOR ( 'NONE', #11009, 1000.000000000000000 ) ;
#18355 = CARTESIAN_POINT ( 'NONE',  ( -67.32681558843928826, 84.01587117655452630, -167.1454815528550739 ) ) ;
#18356 = ORIENTED_EDGE ( 'NONE', *, *, #18288, .F. ) ;
#18357 = DIRECTION ( 'NONE',  ( -1.000000000000000000, 0.000000000000000000, 1.387778780781443703E-16 ) ) ;
#18358 = CARTESIAN_POINT ( 'NONE',  ( -115.7702289486887395, -96.08423613455721579, -5.654315315326000402 ) ) ;
#18359 = VERTEX_POINT ( 'NONE', #6443 ) ;
#18360 = ORIENTED_EDGE ( 'NONE', *, *, #3648, .F. ) ;
#18361 = ORIENTED_EDGE ( 'NONE', *, *, #9867, .F. ) ;
#18362 = AXIS2_PLACEMENT_3D ( 'NONE', #15023, #8005, #9601 ) ;
#18363 = CARTESIAN_POINT ( 'NONE',  ( -68.05062368187118693, 78.23723799236674381, 15.00000000000006928 ) ) ;
#18364 = DIRECTION ( 'NONE',  ( 1.000000000000000000, 0.000000000000000000, 0.000000000000000000 ) ) ;
#18365 = DIRECTION ( 'NONE',  ( -0.000000000000000000, -0.000000000000000000, -1.000000000000000000 ) ) ;
#18366 = EDGE_CURVE ( 'NONE', #12199, #15122, #12163, .T. ) ;
#18367 = LINE ( 'NONE', #2641, #7454 ) ;
#18368 = PLANE ( 'NONE',  #647 ) ;
#18369 = ORIENTED_EDGE ( 'NONE', *, *, #8912, .T. ) ;
#18370 = AXIS2_PLACEMENT_3D ( 'NONE', #2185, #12012, #6288 ) ;
#18371 = PLANE ( 'NONE',  #15276 ) ;
#18372 = ORIENTED_EDGE ( 'NONE', *, *, #15581, .T. ) ;
#18373 = DIRECTION ( 'NONE',  ( -1.000000000000000000, -0.000000000000000000, -0.000000000000000000 ) ) ;
#18374 = DIRECTION ( 'NONE',  ( 0.000000000000000000, -1.000000000000000000, -0.000000000000000000 ) ) ;
#18375 = ORIENTED_EDGE ( 'NONE', *, *, #5207, .T. ) ;
#18376 = AXIS2_PLACEMENT_3D ( 'NONE', #6325, #2034, #7736 ) ;
#18377 = CIRCLE ( 'NONE', #10587, 4.599999999999992539 ) ;
#18378 = DIRECTION ( 'NONE',  ( 0.000000000000000000, 0.000000000000000000, 1.000000000000000000 ) ) ;
#18380 = EDGE_LOOP ( 'NONE', ( #6813, #16761, #12759, #9545 ) ) ;
#18379 = AXIS2_PLACEMENT_3D ( 'NONE', #9077, #15044, #10744 ) ;
#18381 = PRODUCT ( 'Lower Replaceable Die Bushing', 'Lower Replaceable Die Bushing', '', ( #9480 ) ) ;
#18382 = EDGE_CURVE ( 'NONE', #17405, #7351, #1896, .T. ) ;
#18383 = EDGE_LOOP ( 'NONE', ( #13580, #11143, #12512, #4527 ) ) ;
#18384 = AXIS2_PLACEMENT_3D ( 'NONE', #15834, #17583, #295 ) ;
#18385 = PLANE ( 'NONE',  #8455 ) ;
#18386 = AXIS2_PLACEMENT_3D ( 'NONE', #11846, #14560, #10258 ) ;
#18387 = EDGE_LOOP ( 'NONE', ( #2723, #12233, #6206, #11255 ) ) ;
#18388 = ITEM_DEFINED_TRANSFORMATION ( 'NONE', 'NONE', #1001,  #16217 ) ;
#18389 = EDGE_LOOP ( 'NONE', ( #1569, #13341, #13956, #12106 ) ) ;
#18390 = AXIS2_PLACEMENT_3D ( 'NONE', #6923, #9448, #3634 ) ;
#18391 = VECTOR ( 'NONE', #2519, 1000.000000000000000 ) ;
#18392 = CARTESIAN_POINT ( 'NONE',  ( -31.74593505105995916, -91.08423613455721579, 10.65431531532568599 ) ) ;
#18393 = DIRECTION ( 'NONE',  ( -0.9396926207859084279, 0.3420201433256686574, 1.086737899652989892E-16 ) ) ;
#18394 = VERTEX_POINT ( 'NONE', #14033 ) ;
#18395 = PLANE ( 'NONE',  #9905 ) ;
#18396 = DIRECTION ( 'NONE',  ( -2.062304371594500494E-16, 1.000000000000000000, 0.000000000000000000 ) ) ;
#18397 = ORIENTED_EDGE ( 'NONE', *, *, #15790, .T. ) ;
#18398 = FACE_OUTER_BOUND ( 'NONE', #872, .T. ) ;
#18399 = DIRECTION ( 'NONE',  ( -1.000000000000000000, 0.000000000000000000, 0.000000000000000000 ) ) ;
#18400 = ORIENTED_EDGE ( 'NONE', *, *, #4904, .F. ) ;
#18401 = DIRECTION ( 'NONE',  ( 0.3420201433256701007, -0.9396926207859078728, 0.000000000000000000 ) ) ;
#18402 = AXIS2_PLACEMENT_3D ( 'NONE', #13668, #2150, #12172 ) ;
#18403 = CARTESIAN_POINT ( 'NONE',  ( -68.99615306438072082, 139.6252324316626812, 15.00000000000006928 ) ) ;
#18404 = AXIS2_PLACEMENT_3D ( 'NONE', #17371, #16146, #4558 ) ;
#18405 = EDGE_LOOP ( 'NONE', ( #6142, #18283, #9647, #5396 ) ) ;
#18406 = AXIS2_PLACEMENT_3D ( 'NONE', #2027, #5012, #4653 ) ;
#18407 = ADVANCED_FACE ( 'NONE', ( #15433 ), #1123, .F. ) ;
#18408 = ORIENTED_EDGE ( 'NONE', *, *, #18455, .F. ) ;
#18409 = CARTESIAN_POINT ( 'NONE',  ( -68.99615306438120399, -1.746436818337276931, -15.00000000000001421 ) ) ;
#18410 = CARTESIAN_POINT ( 'NONE',  ( -68.99615306438074924, 120.7756765316626542, 15.00000000000006928 ) ) ;
#18411 = ORIENTED_EDGE ( 'NONE', *, *, #8873, .F. ) ;
#18412 = CARTESIAN_POINT ( 'NONE',  ( -51.34465738200551499, 92.72253132893560235, -167.1454815528550739 ) ) ;
#18413 = CARTESIAN_POINT ( 'NONE',  ( -71.24615306438114715, 13.14259340456377956, -167.1454815528550739 ) ) ;
#18414 = FACE_OUTER_BOUND ( 'NONE', #10605, .T. ) ;
#18415 = DIRECTION ( 'NONE',  ( 0.3420201433256519485, 0.9396926207859145341, -0.000000000000000000 ) ) ;
#18416 = ORIENTED_EDGE ( 'NONE', *, *, #10821, .T. ) ;
#18417 = ADVANCED_FACE ( 'NONE', ( #6732 ), #18516, .F. ) ;
#18418 = LINE ( 'NONE', #2963, #11391 ) ;
#18419 = CARTESIAN_POINT ( 'NONE',  ( -71.24615306438076345, 119.0678727652292253, -167.1454815528550739 ) ) ;
#18420 = CARTESIAN_POINT ( 'NONE',  ( 1.801461313472378700, 2.685927156466989096, -49.76172839322247654 ) ) ;
#18421 = DIRECTION ( 'NONE',  ( -0.9396926207859069846, 0.3420201433256723766, 0.000000000000000000 ) ) ;
#18422 = ORIENTED_EDGE ( 'NONE', *, *, #13607, .T. ) ;
#18423 = DIRECTION ( 'NONE',  ( -0.9396926207859092051, 0.3420201433256663259, 1.086737899652990755E-16 ) ) ;
#18424 = DIRECTION ( 'NONE',  ( 0.000000000000000000, 1.000000000000000000, 0.000000000000000000 ) ) ;
#18425 = DIRECTION ( 'NONE',  ( -0.000000000000000000, -0.000000000000000000, -1.000000000000000000 ) ) ;
#18426 = DIRECTION ( 'NONE',  ( 0.3420201433256727097, 0.9396926207859069846, -0.000000000000000000 ) ) ;
#18427 = VERTEX_POINT ( 'NONE', #18434 ) ;
#18428 = EDGE_CURVE ( 'NONE', #11558, #5703, #16827, .T. ) ;
#18429 = ORIENTED_EDGE ( 'NONE', *, *, #16245, .F. ) ;
#18430 = EDGE_CURVE ( 'NONE', #9555, #12621, #8317, .T. ) ;
#18431 = LINE ( 'NONE', #439, #10853 ) ;
#18432 = ORIENTED_EDGE ( 'NONE', *, *, #17259, .T. ) ;
#18433 = DIRECTION ( 'NONE',  ( -0.9396926207859084279, 0.3420201433256686574, -4.890320548438448905E-16 ) ) ;
#18434 = CARTESIAN_POINT ( 'NONE',  ( -51.81614838398844824, 95.01461175692088545, -15.00000000000001421 ) ) ;
#18435 = CARTESIAN_POINT ( 'NONE',  ( -64.29464362790038479, -93.39009773859099539, -44.16867391556240108 ) ) ;
#18436 = VERTEX_POINT ( 'NONE', #3918 ) ;
#18437 = EDGE_CURVE ( 'NONE', #13494, #7683, #4019, .T. ) ;
#18438 = EDGE_CURVE ( 'NONE', #11065, #13894, #5599, .T. ) ;
#18439 = CARTESIAN_POINT ( 'NONE',  ( -68.99615306438070661, 137.0984956381303164, -167.1454815528550739 ) ) ;
#18440 = ADVANCED_FACE ( 'NONE', ( #12452 ), #9628, .T. ) ;
#18441 = CARTESIAN_POINT ( 'NONE',  ( -57.08002265617300708, 84.22855780814606419, -15.00000000000001421 ) ) ;
#18442 = CARTESIAN_POINT ( 'NONE',  ( -36.44155368744861079, 56.74635804676026396, 22.50216374311547440 ) ) ;
#18443 = CARTESIAN_POINT ( 'NONE',  ( -94.45685920050698314, -47.21335801510345220, 15.00000000000006928 ) ) ;
#18444 = VERTEX_POINT ( 'NONE', #11239 ) ;
#18445 = ADVANCED_FACE ( 'NONE', ( #12815 ), #15331, .T. ) ;
#18446 = PLANE ( 'NONE',  #12884 ) ;
#18447 = ORIENTED_EDGE ( 'NONE', *, *, #13860, .T. ) ;
#18448 = ADVANCED_FACE ( 'NONE', ( #16631 ), #3823, .F. ) ;
#18449 = CARTESIAN_POINT ( 'NONE',  ( -127.5926225674731995, 110.5691553257988460, -22.35917033480641791 ) ) ;
#18450 = LINE ( 'NONE', #13021, #11616 ) ;
#18451 = ORIENTED_EDGE ( 'NONE', *, *, #2375, .F. ) ;
#18452 = B_SPLINE_CURVE_WITH_KNOTS ( 'NONE', 3,
 ( #14780, #1975, #7675, #13380, #556, #4857, #10578, #14865, #2056, #7758, #14951, #13475, #656, #17774, #4958, #16359, #3546, #9262, #2146, #7855, #758, #6449, #12169, #17858, #5040, #12459, #15241, #6828 ),
 .UNSPECIFIED., .F., .F.,
 ( 4, 2, 2, 2, 2, 2, 2, 2, 2, 2, 2, 2, 2, 4 ),
 ( 0.000000000000000000, 0.0006831928620949466457, 0.001366385724189893291, 0.001707982155237364229, 0.002049578586284835167, 0.002732771448379764899, 0.003415964310474694197, 0.004099157172569624363, 0.004782350034664553662, 0.005465542896759482960, 0.006831928620949360639, 0.007515121483044319428, 0.008198314345139278217, 0.01093108579351914633 ),
 .UNSPECIFIED. ) ;
#18453 = VERTEX_POINT ( 'NONE', #5686 ) ;
#18454 = EDGE_CURVE ( 'NONE', #13683, #3387, #8230, .T. ) ;
#18455 = EDGE_CURVE ( 'NONE', #1045, #9400, #4113, .T. ) ;
#18456 = VERTEX_POINT ( 'NONE', #12746 ) ;
#18457 = PRODUCT_DEFINITION_CONTEXT ( 'detailed design', #8738, 'design' ) ;
#18458 = CARTESIAN_POINT ( 'NONE',  ( -71.24615306438094819, 69.69126110456375045, -167.1454815528550739 ) ) ;
#18459 = DIRECTION ( 'NONE',  ( 0.000000000000000000, 0.000000000000000000, -1.000000000000000000 ) ) ;
#18460 = DIRECTION ( 'NONE',  ( -5.204170427930409450E-16, 0.000000000000000000, 1.000000000000000000 ) ) ;
#18461 = EDGE_CURVE ( 'NONE', #11084, #2867, #11320, .T. ) ;
#18462 = DIRECTION ( 'NONE',  ( 1.000000000000000000, 0.000000000000000000, 0.000000000000000000 ) ) ;
#18463 = CARTESIAN_POINT ( 'NONE',  ( 0.1061556211655609594, 4.836380039389402086, -4.623144047065641082 ) ) ;
#18464 = VERTEX_POINT ( 'NONE', #2810 ) ;
#18465 = FACE_OUTER_BOUND ( 'NONE', #4601, .T. ) ;
#18466 = ORIENTED_EDGE ( 'NONE', *, *, #10630, .F. ) ;
#18467 = LINE ( 'NONE', #4233, #14152 ) ;
#18468 = CARTESIAN_POINT ( 'NONE',  ( -68.99615306438072082, 133.9569029881302811, -167.1454815528550739 ) ) ;
#18469 = ORIENTED_EDGE ( 'NONE', *, *, #16245, .T. ) ;
#18470 = ORIENTED_EDGE ( 'NONE', *, *, #9042, .F. ) ;
#18471 = ORIENTED_EDGE ( 'NONE', *, *, #17172, .T. ) ;
#18472 = CARTESIAN_POINT ( 'NONE',  ( -67.59262256747319952, 106.9211863004615140, -28.00000000000000355 ) ) ;
#18473 = FACE_OUTER_BOUND ( 'NONE', #17699, .T. ) ;
#18474 = VERTEX_POINT ( 'NONE', #14230 ) ;
#18475 = ORIENTED_EDGE ( 'NONE', *, *, #1162, .F. ) ;
#18476 = CARTESIAN_POINT ( 'NONE',  ( -212.2032458117903104, 84.22855780814606419, 62.50000000000001421 ) ) ;
#18477 = CARTESIAN_POINT ( 'NONE',  ( -68.99615306438077766, 118.2489397381302751, -15.00000000000001421 ) ) ;
#18478 = VERTEX_POINT ( 'NONE', #1406 ) ;
#18479 = DIRECTION ( 'NONE',  ( -1.000000000000000000, 0.000000000000000000, 0.000000000000000000 ) ) ;
#18480 = CARTESIAN_POINT ( 'NONE',  ( -57.08002265617300708, 84.22855780814606419, 15.00000000000006928 ) ) ;
#18481 = LINE ( 'NONE', #8285, #2794 ) ;
#18482 = VERTEX_POINT ( 'NONE', #4552 ) ;
#18483 = VECTOR ( 'NONE', #10769, 1000.000000000000000 ) ;
#18484 = FACE_OUTER_BOUND ( 'NONE', #3887, .T. ) ;
#18485 = B_SPLINE_CURVE_WITH_KNOTS ( 'NONE', 3,
 ( #16422, #16523, #15028, #3721, #2306, #16619, #3812, #9514, #6323, #12051, #17749, #1114, #3901, #9607, #4287, #16910, #18226, #8304, #6901, #9713, #1471, #15422, #7178, #2888, #17093, #14114, #14018, #1302, #1391, #18132 ),
 .UNSPECIFIED., .F., .F.,
 ( 4, 2, 2, 2, 2, 2, 2, 2, 2, 2, 2, 2, 2, 2, 4 ),
 ( 0.01212337847808446674, 0.02493713703494332412, 0.02814057667415803543, 0.03134401631337273980, 0.03775089559180216936, 0.05056465414866103542, 0.05376809378787574673, 0.05697153342709045803, 0.06337841270551984596, 0.07619217126237863569, 0.08259905054080803055, 0.08580249018002272798, 0.08900592981923741154, 0.1018196883760962013, 0.1146334469329549632 ),
 .UNSPECIFIED. ) ;
#18486 = VERTEX_POINT ( 'NONE', #14656 ) ;
#18487 = EDGE_CURVE ( 'NONE', #889, #9668, #17408, .T. ) ;
#18488 = DIRECTION ( 'NONE',  ( -1.000000000000000000, -0.000000000000000000, -0.000000000000000000 ) ) ;
#18489 = VERTEX_POINT ( 'NONE', #86 ) ;
#18490 = AXIS2_PLACEMENT_3D ( 'NONE', #11125, #8307, #11311 ) ;
#18491 = ORIENTED_EDGE ( 'NONE', *, *, #18089, .T. ) ;
#18492 = ORIENTED_EDGE ( 'NONE', *, *, #5514, .T. ) ;
#18493 = CARTESIAN_POINT ( 'NONE',  ( -80.43148536604020649, 78.95224028009165806, 97.49999999999998579 ) ) ;
#18494 = ORIENTED_EDGE ( 'NONE', *, *, #12204, .F. ) ;
#18495 = DIRECTION ( 'NONE',  ( 1.000000000000000000, 0.000000000000000000, 0.000000000000000000 ) ) ;
#18496 = CARTESIAN_POINT ( 'NONE',  ( 4.699999999999995737, -3.752776749732712691, -6.500000000000033751 ) ) ;
#18497 = CARTESIAN_POINT ( 'NONE',  ( -71.24615306438069240, 141.9478920545637664, -15.00000000000001421 ) ) ;
#18498 = DIRECTION ( 'NONE',  ( -5.204170427930409450E-16, 0.000000000000000000, 1.000000000000000000 ) ) ;
#18499 = ORIENTED_EDGE ( 'NONE', *, *, #8192, .T. ) ;
#18500 = CARTESIAN_POINT ( 'NONE',  ( -71.24615306438106188, 37.38646386522923137, -167.1454815528550739 ) ) ;
#18501 = AXIS2_PLACEMENT_3D ( 'NONE', #8144, #12463, #16552 ) ;
#18502 = CARTESIAN_POINT ( 'NONE',  ( 4.699999999999995737, 6.499999999999901412, 2.428612866367529932E-14 ) ) ;
#18503 = CARTESIAN_POINT ( 'NONE',  ( -83.12361985383351737, 84.22855780814606419, 35.00000000000000000 ) ) ;
#18504 = ORIENTED_EDGE ( 'NONE', *, *, #4473, .F. ) ;
#18505 = CARTESIAN_POINT ( 'NONE',  ( -71.24615306438076345, 119.0678727652292253, -15.00000000000001421 ) ) ;
#18506 = CARTESIAN_POINT ( 'NONE',  ( 9.543663295069050534, 56.41207303426870112, -3.000000000000000000 ) ) ;
#18507 = CARTESIAN_POINT ( 'NONE',  ( -171.0109138863553824, 84.22855780814606419, 55.00000000000000711 ) ) ;
#18508 = CARTESIAN_POINT ( 'NONE',  ( -98.90286936182226896, -91.08423613455721579, -10.65431531532588316 ) ) ;
#18509 = VERTEX_POINT ( 'NONE', #259 ) ;
#18510 = ORIENTED_EDGE ( 'NONE', *, *, #11249, .F. ) ;
#18511 = ADVANCED_FACE ( 'NONE', ( #15723 ), #8686, .T. ) ;
#18512 = VECTOR ( 'NONE', #8627, 1000.000000000000000 ) ;
#18513 = CARTESIAN_POINT ( 'NONE',  ( 0.000000000000000000, -5.629165124598996428, -3.250000000000020428 ) ) ;
#18514 = ORIENTED_EDGE ( 'NONE', *, *, #5280, .F. ) ;
#18515 = VECTOR ( 'NONE', #16988, 999.9999999999998863 ) ;
#18516 = PLANE ( 'NONE',  #4283 ) ;
#18517 = CARTESIAN_POINT ( 'NONE',  ( -68.99615306438094819, 64.22700883166265839, -167.1454815528550739 ) ) ;
#18518 = ORIENTED_EDGE ( 'NONE', *, *, #10577, .F. ) ;
#18519 = ORIENTED_EDGE ( 'NONE', *, *, #3999, .F. ) ;
#18520 = NEXT_ASSEMBLY_USAGE_OCCURRENCE ( 'NAUO1', ' ', ' ', #1557, #6568, $ ) ;
#18521 = NEXT_ASSEMBLY_USAGE_OCCURRENCE ( 'NAUO2', ' ', ' ', #1557, #4980, $ ) ;
#18522 = NEXT_ASSEMBLY_USAGE_OCCURRENCE ( 'NAUO3', ' ', ' ', #1557, #7481, $ ) ;
#18523 = NEXT_ASSEMBLY_USAGE_OCCURRENCE ( 'NAUO4', ' ', ' ', #1557, #13786, $ ) ;
#18524 = NEXT_ASSEMBLY_USAGE_OCCURRENCE ( 'NAUO5', ' ', ' ', #1557, #11622, $ ) ;
#18525 = NEXT_ASSEMBLY_USAGE_OCCURRENCE ( 'NAUO6', ' ', ' ', #1557, #2227, $ ) ;
#18526 = NEXT_ASSEMBLY_USAGE_OCCURRENCE ( 'NAUO7', ' ', ' ', #1557, #7385, $ ) ;
#18527 = NEXT_ASSEMBLY_USAGE_OCCURRENCE ( 'NAUO8', ' ', ' ', #1557, #15399, $ ) ;
#18528 = NEXT_ASSEMBLY_USAGE_OCCURRENCE ( 'NAUO9', ' ', ' ', #1557, #3491, $ ) ;
#18529 = NEXT_ASSEMBLY_USAGE_OCCURRENCE ( 'NAUO10', ' ', ' ', #1557, #3491, $ ) ;
#18530 = NEXT_ASSEMBLY_USAGE_OCCURRENCE ( 'NAUO11', ' ', ' ', #1557, #3491, $ ) ;
#18531 = NEXT_ASSEMBLY_USAGE_OCCURRENCE ( 'NAUO12', ' ', ' ', #1557, #3491, $ ) ;
#18532=COLOUR_RGB('Dark Blue',0.08,0.2,0.34);
#18533=FILL_AREA_STYLE_COLOUR('',#18532);
#18534=FILL_AREA_STYLE('',(#18533));
#18535=SURFACE_STYLE_FILL_AREA(#18534);
#18536=SURFACE_SIDE_STYLE('',(#18535));
#18537=SURFACE_STYLE_USAGE(.BOTH.,#18536);
#18538=PRESENTATION_STYLE_ASSIGNMENT((#18537));
#18539=COLOUR_RGB('Light Blue',0.38,0.62,0.78);
#18540=FILL_AREA_STYLE_COLOUR('',#18539);
#18541=FILL_AREA_STYLE('',(#18540));
#18542=SURFACE_STYLE_FILL_AREA(#18541);
#18543=SURFACE_SIDE_STYLE('',(#18542));
#18544=SURFACE_STYLE_USAGE(.BOTH.,#18543);
#18545=PRESENTATION_STYLE_ASSIGNMENT((#18544));
#18546=COLOUR_RGB('Sky Blue',0.24,0.69,0.87);
#18547=FILL_AREA_STYLE_COLOUR('',#18546);
#18548=FILL_AREA_STYLE('',(#18547));
#18549=SURFACE_STYLE_FILL_AREA(#18548);
#18550=SURFACE_SIDE_STYLE('',(#18549));
#18551=SURFACE_STYLE_USAGE(.BOTH.,#18550);
#18552=PRESENTATION_STYLE_ASSIGNMENT((#18551));
#18553=COLOUR_RGB('Grey',0.48,0.52,0.57);
#18554=FILL_AREA_STYLE_COLOUR('',#18553);
#18555=FILL_AREA_STYLE('',(#18554));
#18556=SURFACE_STYLE_FILL_AREA(#18555);
#18557=SURFACE_SIDE_STYLE('',(#18556));
#18558=SURFACE_STYLE_USAGE(.BOTH.,#18557);
#18559=PRESENTATION_STYLE_ASSIGNMENT((#18558));
#18560=COLOUR_RGB('Black',0.12,0.14,0.17);
#18561=FILL_AREA_STYLE_COLOUR('',#18560);
#18562=FILL_AREA_STYLE('',(#18561));
#18563=SURFACE_STYLE_FILL_AREA(#18562);
#18564=SURFACE_SIDE_STYLE('',(#18563));
#18565=SURFACE_STYLE_USAGE(.BOTH.,#18564);
#18566=PRESENTATION_STYLE_ASSIGNMENT((#18565));
#18567=COLOUR_RGB('Off White',0.89,0.88,0.83);
#18568=FILL_AREA_STYLE_COLOUR('',#18567);
#18569=FILL_AREA_STYLE('',(#18568));
#18570=SURFACE_STYLE_FILL_AREA(#18569);
#18571=SURFACE_SIDE_STYLE('',(#18570));
#18572=SURFACE_STYLE_USAGE(.BOTH.,#18571);
#18573=PRESENTATION_STYLE_ASSIGNMENT((#18572));
ENDSEC;
END-ISO-10303-21;
